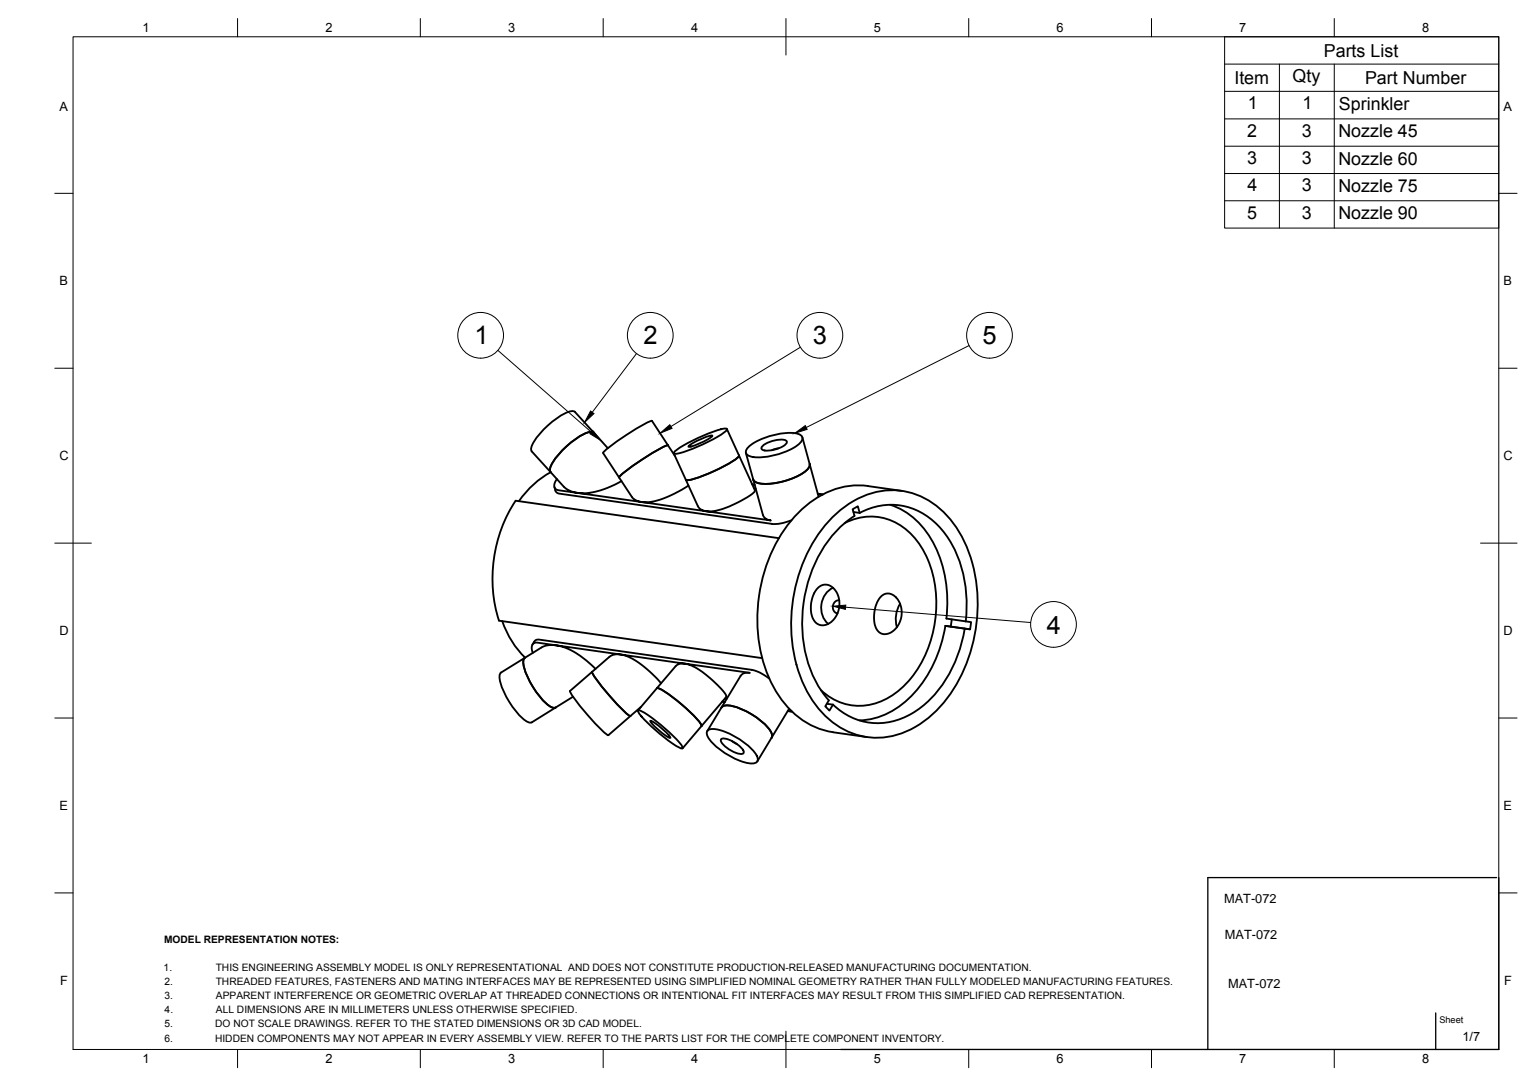
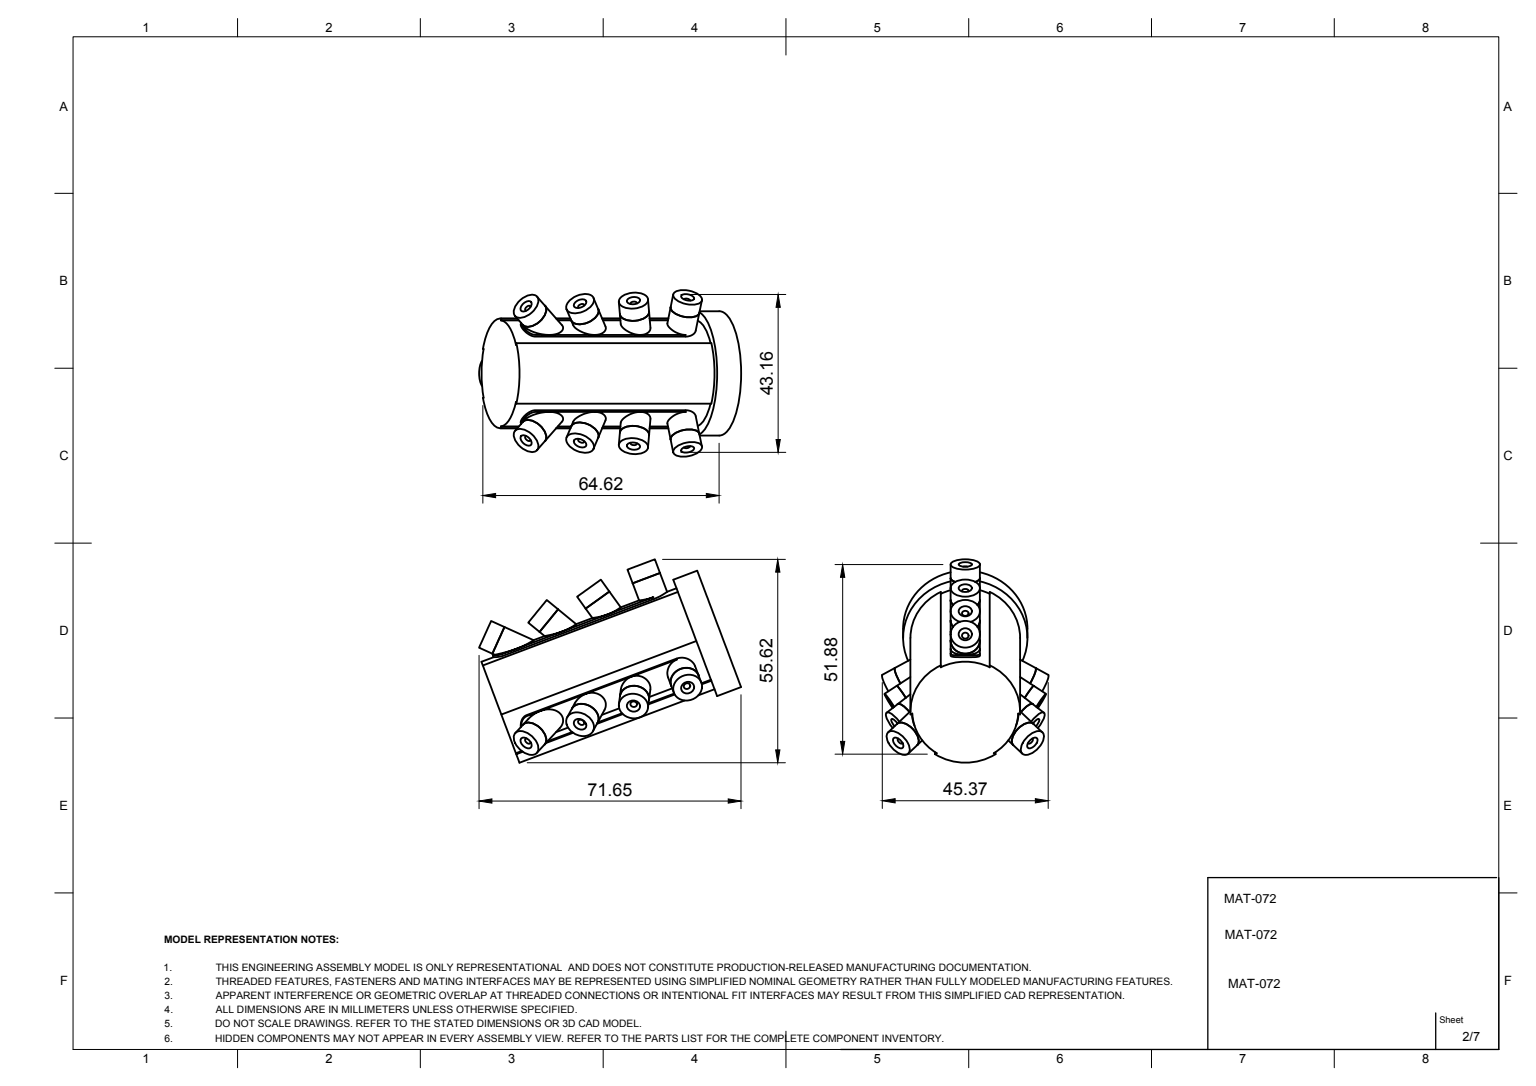
ISO-10303-21;
HEADER;
/* Generated by software containing ST-Developer
 * from STEP Tools, Inc. (www.steptools.com) 
 */

FILE_DESCRIPTION(
/* description */ (''),
/* implementation_level */ '2;1');

FILE_NAME(
/* name */ 'MAT-072',
/* time_stamp */ '2026-10-24T10:30:45-07:00',
/* author */ (''),
/* organization */ (''),
/* preprocessor_version */ 'ST-DEVELOPER v20.2',
/* originating_system */ 'Autodesk Translation Framework v15.15.0.0',
/* authorisation */ '');

FILE_SCHEMA (('AUTOMOTIVE_DESIGN { 1 0 10303 214 3 1 1 }'));
ENDSEC;

DATA;
#10=MECHANICAL_DESIGN_GEOMETRIC_PRESENTATION_REPRESENTATION('',(#77,#78,
#79,#80,#81),#5183);
#11=ITEM_DEFINED_TRANSFORMATION($,$,#2425,#2665);
#12=ITEM_DEFINED_TRANSFORMATION($,$,#2605,#2666);
#13=ITEM_DEFINED_TRANSFORMATION($,$,#2620,#2667);
#14=ITEM_DEFINED_TRANSFORMATION($,$,#2635,#2668);
#15=ITEM_DEFINED_TRANSFORMATION($,$,#2650,#2669);
#16=ITEM_DEFINED_TRANSFORMATION($,$,#2605,#2670);
#17=ITEM_DEFINED_TRANSFORMATION($,$,#2605,#2671);
#18=ITEM_DEFINED_TRANSFORMATION($,$,#2620,#2672);
#19=ITEM_DEFINED_TRANSFORMATION($,$,#2620,#2673);
#20=ITEM_DEFINED_TRANSFORMATION($,$,#2635,#2674);
#21=ITEM_DEFINED_TRANSFORMATION($,$,#2635,#2675);
#22=ITEM_DEFINED_TRANSFORMATION($,$,#2650,#2676);
#23=ITEM_DEFINED_TRANSFORMATION($,$,#2650,#2677);
#24=(
REPRESENTATION_RELATIONSHIP($,$,#5214,#5213)
REPRESENTATION_RELATIONSHIP_WITH_TRANSFORMATION(#11)
SHAPE_REPRESENTATION_RELATIONSHIP()
);
#25=(
REPRESENTATION_RELATIONSHIP($,$,#5215,#5213)
REPRESENTATION_RELATIONSHIP_WITH_TRANSFORMATION(#12)
SHAPE_REPRESENTATION_RELATIONSHIP()
);
#26=(
REPRESENTATION_RELATIONSHIP($,$,#5216,#5213)
REPRESENTATION_RELATIONSHIP_WITH_TRANSFORMATION(#13)
SHAPE_REPRESENTATION_RELATIONSHIP()
);
#27=(
REPRESENTATION_RELATIONSHIP($,$,#5217,#5213)
REPRESENTATION_RELATIONSHIP_WITH_TRANSFORMATION(#14)
SHAPE_REPRESENTATION_RELATIONSHIP()
);
#28=(
REPRESENTATION_RELATIONSHIP($,$,#5218,#5213)
REPRESENTATION_RELATIONSHIP_WITH_TRANSFORMATION(#15)
SHAPE_REPRESENTATION_RELATIONSHIP()
);
#29=(
REPRESENTATION_RELATIONSHIP($,$,#5215,#5213)
REPRESENTATION_RELATIONSHIP_WITH_TRANSFORMATION(#16)
SHAPE_REPRESENTATION_RELATIONSHIP()
);
#30=(
REPRESENTATION_RELATIONSHIP($,$,#5215,#5213)
REPRESENTATION_RELATIONSHIP_WITH_TRANSFORMATION(#17)
SHAPE_REPRESENTATION_RELATIONSHIP()
);
#31=(
REPRESENTATION_RELATIONSHIP($,$,#5216,#5213)
REPRESENTATION_RELATIONSHIP_WITH_TRANSFORMATION(#18)
SHAPE_REPRESENTATION_RELATIONSHIP()
);
#32=(
REPRESENTATION_RELATIONSHIP($,$,#5216,#5213)
REPRESENTATION_RELATIONSHIP_WITH_TRANSFORMATION(#19)
SHAPE_REPRESENTATION_RELATIONSHIP()
);
#33=(
REPRESENTATION_RELATIONSHIP($,$,#5217,#5213)
REPRESENTATION_RELATIONSHIP_WITH_TRANSFORMATION(#20)
SHAPE_REPRESENTATION_RELATIONSHIP()
);
#34=(
REPRESENTATION_RELATIONSHIP($,$,#5217,#5213)
REPRESENTATION_RELATIONSHIP_WITH_TRANSFORMATION(#21)
SHAPE_REPRESENTATION_RELATIONSHIP()
);
#35=(
REPRESENTATION_RELATIONSHIP($,$,#5218,#5213)
REPRESENTATION_RELATIONSHIP_WITH_TRANSFORMATION(#22)
SHAPE_REPRESENTATION_RELATIONSHIP()
);
#36=(
REPRESENTATION_RELATIONSHIP($,$,#5218,#5213)
REPRESENTATION_RELATIONSHIP_WITH_TRANSFORMATION(#23)
SHAPE_REPRESENTATION_RELATIONSHIP()
);
#37=CONTEXT_DEPENDENT_SHAPE_REPRESENTATION(#24,#5200);
#38=CONTEXT_DEPENDENT_SHAPE_REPRESENTATION(#25,#5201);
#39=CONTEXT_DEPENDENT_SHAPE_REPRESENTATION(#26,#5202);
#40=CONTEXT_DEPENDENT_SHAPE_REPRESENTATION(#27,#5203);
#41=CONTEXT_DEPENDENT_SHAPE_REPRESENTATION(#28,#5204);
#42=CONTEXT_DEPENDENT_SHAPE_REPRESENTATION(#29,#5205);
#43=CONTEXT_DEPENDENT_SHAPE_REPRESENTATION(#30,#5206);
#44=CONTEXT_DEPENDENT_SHAPE_REPRESENTATION(#31,#5207);
#45=CONTEXT_DEPENDENT_SHAPE_REPRESENTATION(#32,#5208);
#46=CONTEXT_DEPENDENT_SHAPE_REPRESENTATION(#33,#5209);
#47=CONTEXT_DEPENDENT_SHAPE_REPRESENTATION(#34,#5210);
#48=CONTEXT_DEPENDENT_SHAPE_REPRESENTATION(#35,#5211);
#49=CONTEXT_DEPENDENT_SHAPE_REPRESENTATION(#36,#5212);
#50=NEXT_ASSEMBLY_USAGE_OCCURRENCE('Sprinkler:1','Sprinkler:1',
'Sprinkler:1',#5220,#5221,'Sprinkler:1');
#51=NEXT_ASSEMBLY_USAGE_OCCURRENCE('Nozzle 45:1','Nozzle 45:1',
'Nozzle 45:1',#5220,#5222,'Nozzle 45:1');
#52=NEXT_ASSEMBLY_USAGE_OCCURRENCE('Nozzle 60:1','Nozzle 60:1',
'Nozzle 60:1',#5220,#5223,'Nozzle 60:1');
#53=NEXT_ASSEMBLY_USAGE_OCCURRENCE('Nozzle 75:1','Nozzle 75:1',
'Nozzle 75:1',#5220,#5224,'Nozzle 75:1');
#54=NEXT_ASSEMBLY_USAGE_OCCURRENCE('Nozzle 90:1','Nozzle 90:1',
'Nozzle 90:1',#5220,#5225,'Nozzle 90:1');
#55=NEXT_ASSEMBLY_USAGE_OCCURRENCE('Nozzle 45:2','Nozzle 45:2',
'Nozzle 45:2',#5220,#5222,'Nozzle 45:2');
#56=NEXT_ASSEMBLY_USAGE_OCCURRENCE('Nozzle 45:3','Nozzle 45:3',
'Nozzle 45:3',#5220,#5222,'Nozzle 45:3');
#57=NEXT_ASSEMBLY_USAGE_OCCURRENCE('Nozzle 60:2','Nozzle 60:2',
'Nozzle 60:2',#5220,#5223,'Nozzle 60:2');
#58=NEXT_ASSEMBLY_USAGE_OCCURRENCE('Nozzle 60:3','Nozzle 60:3',
'Nozzle 60:3',#5220,#5223,'Nozzle 60:3');
#59=NEXT_ASSEMBLY_USAGE_OCCURRENCE('Nozzle 75:2','Nozzle 75:2',
'Nozzle 75:2',#5220,#5224,'Nozzle 75:2');
#60=NEXT_ASSEMBLY_USAGE_OCCURRENCE('Nozzle 75:3','Nozzle 75:3',
'Nozzle 75:3',#5220,#5224,'Nozzle 75:3');
#61=NEXT_ASSEMBLY_USAGE_OCCURRENCE('Nozzle 90:2','Nozzle 90:2',
'Nozzle 90:2',#5220,#5225,'Nozzle 90:2');
#62=NEXT_ASSEMBLY_USAGE_OCCURRENCE('Nozzle 90:3','Nozzle 90:3',
'Nozzle 90:3',#5220,#5225,'Nozzle 90:3');
#63=CONICAL_SURFACE('',#2616,1.8,0.785398163397447);
#64=CONICAL_SURFACE('',#2631,1.8,0.785398163397439);
#65=CONICAL_SURFACE('',#2646,1.80000000000001,0.785398163397454);
#66=CONICAL_SURFACE('',#2661,1.8,0.785398163397448);
#67=SHAPE_REPRESENTATION_RELATIONSHIP('SRR','None',#5214,#72);
#68=SHAPE_REPRESENTATION_RELATIONSHIP('SRR','None',#5215,#73);
#69=SHAPE_REPRESENTATION_RELATIONSHIP('SRR','None',#5216,#74);
#70=SHAPE_REPRESENTATION_RELATIONSHIP('SRR','None',#5217,#75);
#71=SHAPE_REPRESENTATION_RELATIONSHIP('SRR','None',#5218,#76);
#72=ADVANCED_BREP_SHAPE_REPRESENTATION('',(#82),#5178);
#73=ADVANCED_BREP_SHAPE_REPRESENTATION('',(#83),#5179);
#74=ADVANCED_BREP_SHAPE_REPRESENTATION('',(#84),#5180);
#75=ADVANCED_BREP_SHAPE_REPRESENTATION('',(#85),#5181);
#76=ADVANCED_BREP_SHAPE_REPRESENTATION('',(#86),#5182);
#77=STYLED_ITEM('',(#5247),#82);
#78=STYLED_ITEM('',(#5247),#83);
#79=STYLED_ITEM('',(#5247),#84);
#80=STYLED_ITEM('',(#5247),#85);
#81=STYLED_ITEM('',(#5247),#86);
#82=MANIFOLD_SOLID_BREP('Sprinkler',#2363);
#83=MANIFOLD_SOLID_BREP('Nozzle 45',#2364);
#84=MANIFOLD_SOLID_BREP('Nozzle 60',#2365);
#85=MANIFOLD_SOLID_BREP('Nozzle 75',#2366);
#86=MANIFOLD_SOLID_BREP('Nozzle 90',#2367);
#87=B_SPLINE_SURFACE_WITH_KNOTS('',3,1,((#4861,#4862),(#4863,#4864),(#4865,
#4866),(#4867,#4868),(#4869,#4870),(#4871,#4872),(#4873,#4874),(#4875,#4876),
(#4877,#4878),(#4879,#4880),(#4881,#4882)),.UNSPECIFIED.,.F.,.F.,.F.,(4,
1,1,1,1,1,1,1,4),(2,2),(3.14159265358979,3.53429173528852,3.92699081698724,
4.31968989868597,4.71238898038469,5.10508806208341,5.49778714378214,5.89048622548086,
6.28318530717959),(0.,0.129347179873149),.UNSPECIFIED.);
#88=B_SPLINE_SURFACE_WITH_KNOTS('',3,1,((#4924,#4925),(#4926,#4927),(#4928,
#4929),(#4930,#4931),(#4932,#4933),(#4934,#4935),(#4936,#4937),(#4938,#4939),
(#4940,#4941),(#4942,#4943),(#4944,#4945)),.UNSPECIFIED.,.F.,.F.,.F.,(4,
1,1,1,1,1,1,1,4),(2,2),(3.14159265358979,3.53429173528851,3.92699081698724,
4.31968989868596,4.71238898038469,5.10508806208341,5.49778714378214,5.89048622548086,
6.28318530717959),(0.,0.129347179873148),.UNSPECIFIED.);
#89=B_SPLINE_SURFACE_WITH_KNOTS('',3,1,((#4987,#4988),(#4989,#4990),(#4991,
#4992),(#4993,#4994),(#4995,#4996),(#4997,#4998),(#4999,#5000),(#5001,#5002),
(#5003,#5004),(#5005,#5006),(#5007,#5008)),.UNSPECIFIED.,.F.,.F.,.F.,(4,
1,1,1,1,1,1,1,4),(2,2),(3.14159265358979,3.53429173528851,3.92699081698723,
4.31968989868596,4.71238898038468,5.10508806208341,5.49778714378213,5.89048622548085,
6.28318530717958),(0.,0.129347179873145),.UNSPECIFIED.);
#90=FACE_BOUND('',#431,.T.);
#91=FACE_BOUND('',#433,.T.);
#92=FACE_BOUND('',#436,.T.);
#93=FACE_BOUND('',#439,.T.);
#94=FACE_BOUND('',#442,.T.);
#95=FACE_BOUND('',#445,.T.);
#96=FACE_BOUND('',#448,.T.);
#97=FACE_BOUND('',#451,.T.);
#98=FACE_BOUND('',#454,.T.);
#99=FACE_BOUND('',#457,.T.);
#100=FACE_BOUND('',#460,.T.);
#101=FACE_BOUND('',#461,.T.);
#102=FACE_BOUND('',#462,.T.);
#103=FACE_BOUND('',#463,.T.);
#104=FACE_BOUND('',#464,.T.);
#105=FACE_BOUND('',#465,.T.);
#106=FACE_BOUND('',#466,.T.);
#107=FACE_BOUND('',#467,.T.);
#108=FACE_BOUND('',#468,.T.);
#109=FACE_BOUND('',#469,.T.);
#110=FACE_BOUND('',#470,.T.);
#111=FACE_BOUND('',#471,.T.);
#112=FACE_BOUND('',#474,.T.);
#113=FACE_BOUND('',#481,.T.);
#114=FACE_BOUND('',#484,.T.);
#115=FACE_BOUND('',#487,.T.);
#116=FACE_BOUND('',#490,.T.);
#117=FACE_BOUND('',#493,.T.);
#118=FACE_BOUND('',#496,.T.);
#119=FACE_BOUND('',#499,.T.);
#120=FACE_BOUND('',#502,.T.);
#121=FACE_BOUND('',#513,.T.);
#122=FACE_BOUND('',#516,.T.);
#123=FACE_BOUND('',#519,.T.);
#124=FACE_BOUND('',#522,.T.);
#125=FACE_BOUND('',#525,.T.);
#126=FACE_BOUND('',#528,.T.);
#127=FACE_BOUND('',#531,.T.);
#128=FACE_BOUND('',#534,.T.);
#129=FACE_BOUND('',#542,.T.);
#130=FACE_BOUND('',#549,.T.);
#131=FACE_BOUND('',#556,.T.);
#132=FACE_BOUND('',#568,.T.);
#133=FACE_BOUND('',#570,.T.);
#134=FACE_BOUND('',#574,.T.);
#135=FACE_BOUND('',#578,.T.);
#136=FACE_BOUND('',#580,.T.);
#137=FACE_BOUND('',#584,.T.);
#138=FACE_BOUND('',#588,.T.);
#139=FACE_BOUND('',#590,.T.);
#140=FACE_BOUND('',#594,.T.);
#141=FACE_BOUND('',#598,.T.);
#142=FACE_BOUND('',#600,.T.);
#143=FACE_BOUND('',#604,.T.);
#144=PLANE('',#2456);
#145=PLANE('',#2461);
#146=PLANE('',#2464);
#147=PLANE('',#2466);
#148=PLANE('',#2470);
#149=PLANE('',#2474);
#150=PLANE('',#2478);
#151=PLANE('',#2482);
#152=PLANE('',#2486);
#153=PLANE('',#2490);
#154=PLANE('',#2494);
#155=PLANE('',#2500);
#156=PLANE('',#2501);
#157=PLANE('',#2509);
#158=PLANE('',#2513);
#159=PLANE('',#2517);
#160=PLANE('',#2521);
#161=PLANE('',#2525);
#162=PLANE('',#2529);
#163=PLANE('',#2533);
#164=PLANE('',#2537);
#165=PLANE('',#2557);
#166=PLANE('',#2560);
#167=PLANE('',#2563);
#168=PLANE('',#2566);
#169=PLANE('',#2569);
#170=PLANE('',#2572);
#171=PLANE('',#2575);
#172=PLANE('',#2578);
#173=PLANE('',#2581);
#174=PLANE('',#2582);
#175=PLANE('',#2583);
#176=PLANE('',#2584);
#177=PLANE('',#2586);
#178=PLANE('',#2587);
#179=PLANE('',#2588);
#180=PLANE('',#2589);
#181=PLANE('',#2591);
#182=PLANE('',#2592);
#183=PLANE('',#2593);
#184=PLANE('',#2594);
#185=PLANE('',#2596);
#186=PLANE('',#2597);
#187=PLANE('',#2598);
#188=PLANE('',#2599);
#189=PLANE('',#2600);
#190=PLANE('',#2601);
#191=PLANE('',#2602);
#192=PLANE('',#2603);
#193=PLANE('',#2604);
#194=PLANE('',#2609);
#195=PLANE('',#2611);
#196=PLANE('',#2617);
#197=PLANE('',#2624);
#198=PLANE('',#2626);
#199=PLANE('',#2632);
#200=PLANE('',#2639);
#201=PLANE('',#2641);
#202=PLANE('',#2647);
#203=PLANE('',#2654);
#204=PLANE('',#2656);
#205=PLANE('',#2662);
#206=B_SPLINE_CURVE_WITH_KNOTS('',3,(#3370,#3371,#3372,#3373,#3374,#3375,
#3376,#3377),.UNSPECIFIED.,.F.,.F.,(4,2,2,4),(0.801601659973552,0.908686694681274,
1.06147652934293,1.21426636400458),.UNSPECIFIED.);
#207=B_SPLINE_CURVE_WITH_KNOTS('',3,(#3379,#3380,#3381,#3382,#3383,#3384,
#3385,#3386,#3387,#3388,#3389,#3390,#3391,#3392),.UNSPECIFIED.,.F.,.F.,
(4,2,2,2,2,2,4),(0.,0.152789834661652,0.305579669323305,0.456356425662796,
0.607133182002287,0.757909938341781,0.801601659973552),.UNSPECIFIED.);
#208=B_SPLINE_CURVE_WITH_KNOTS('',3,(#3396,#3397,#3398,#3399,#3400,#3401,
#3402,#3403,#3404,#3405,#3406,#3407,#3408,#3409,#3410,#3411),
 .UNSPECIFIED.,.F.,.F.,(4,2,2,2,2,2,2,4),(1.41258149283994,1.51470567835646,
1.66615965590029,1.81761363344413,1.96906761098797,2.12052158853181,2.27200321656199,
2.42348484459217),.UNSPECIFIED.);
#209=B_SPLINE_CURVE_WITH_KNOTS('',3,(#3412,#3413,#3414,#3415,#3416,#3417),
 .UNSPECIFIED.,.F.,.F.,(4,2,4),(1.21174242229609,1.36322405032627,1.41258149283994),
 .UNSPECIFIED.);
#210=B_SPLINE_CURVE_WITH_KNOTS('',3,(#3422,#3423,#3424,#3425,#3426,#3427,
#3428,#3429),.UNSPECIFIED.,.F.,.F.,(4,2,2,4),(0.810459053731311,0.931112082660273,
1.09792489409666,1.26473770553305),.UNSPECIFIED.);
#211=B_SPLINE_CURVE_WITH_KNOTS('',3,(#3431,#3432,#3433,#3434,#3435,#3436,
#3437,#3438,#3439,#3440,#3441,#3442,#3443,#3444),.UNSPECIFIED.,.F.,.F.,
(4,2,2,2,2,2,4),(0.,0.166812811436392,0.333625622872784,0.482997237819655,
0.632368852766526,0.781740467713401,0.810459053731311),.UNSPECIFIED.);
#212=B_SPLINE_CURVE_WITH_KNOTS('',3,(#3446,#3447,#3448,#3449,#3450,#3451,
#3452,#3453,#3454,#3455,#3456,#3457,#3458,#3459,#3460,#3461,#3462,#3463),
 .UNSPECIFIED.,.F.,.F.,(4,2,2,2,2,2,2,2,4),(1.21426636400458,1.37281902636882,
1.53137168873306,1.68587949128402,1.84038729383497,1.99489509638593,2.14940289893689,
2.30795556130114,2.46650822366539),.UNSPECIFIED.);
#213=B_SPLINE_CURVE_WITH_KNOTS('',3,(#3468,#3469,#3470,#3471,#3472,#3473,
#3474,#3475,#3476,#3477),.UNSPECIFIED.,.F.,.F.,(4,2,2,2,4),(0.84921255840186,
0.855460999411689,1.0133776521287,1.20423317275903,1.39508869338936),
 .UNSPECIFIED.);
#214=B_SPLINE_CURVE_WITH_KNOTS('',3,(#3479,#3480,#3481,#3482,#3483,#3484,
#3485,#3486,#3487,#3488,#3489,#3490),.UNSPECIFIED.,.F.,.F.,(4,2,2,2,2,4),
(0.,0.19085552063033,0.38171104126066,0.539627693977667,0.697544346694674,
0.84921255840186),.UNSPECIFIED.);
#215=B_SPLINE_CURVE_WITH_KNOTS('',3,(#3492,#3493,#3494,#3495,#3496,#3497,
#3498,#3499,#3500,#3501,#3502,#3503,#3504,#3505,#3506,#3507,#3508,#3509),
 .UNSPECIFIED.,.F.,.F.,(4,2,2,2,2,2,2,2,4),(1.26473770553305,1.44115993597425,
1.61758216641546,1.77878219205947,1.93998221770349,2.10118224334752,2.26238226899155,
2.43880449943275,2.61522672987395),.UNSPECIFIED.);
#216=B_SPLINE_CURVE_WITH_KNOTS('',3,(#3513,#3514,#3515,#3516,#3517,#3518,
#3519,#3520,#3521,#3522,#3523,#3524,#3525,#3526,#3527,#3528,#3529,#3530,
#3531,#3532,#3533,#3534),.UNSPECIFIED.,.F.,.F.,(4,2,2,2,2,2,2,2,2,2,4),
(1.39508869338936,1.63068735474474,1.86628601610013,2.01895939966093,2.09529609144134,
2.17163278322174,2.24796947500215,2.32430616678255,2.47697955034337,2.71257821169876,
2.94817687305416),.UNSPECIFIED.);
#217=B_SPLINE_CURVE_WITH_KNOTS('',3,(#3537,#3538,#3539,#3540,#3541,#3542,
#3543,#3544,#3545,#3546,#3547,#3548,#3549,#3550,#3551,#3552,#3553,#3554,
#3555,#3556,#3557,#3558,#3559,#3560,#3561,#3562),.UNSPECIFIED.,.F.,.F.,
(4,2,2,2,2,2,2,2,2,2,2,2,4),(0.,0.0444658256706816,0.109825747467382,0.210987273969983,
0.363115011869221,0.476603266918211,0.543343022865724,0.610052308554092,
0.7232875236507,0.87579543247345,0.97697424211648,1.04237097445545,1.08685368328188),
 .UNSPECIFIED.);
#218=B_SPLINE_CURVE_WITH_KNOTS('',3,(#3577,#3578,#3579,#3580,#3581,#3582,
#3583,#3584),.UNSPECIFIED.,.F.,.F.,(4,2,2,4),(0.801601659973551,0.908686694681269,
1.06147652934292,1.21426636400457),.UNSPECIFIED.);
#219=B_SPLINE_CURVE_WITH_KNOTS('',3,(#3586,#3587,#3588,#3589,#3590,#3591,
#3592,#3593,#3594,#3595,#3596,#3597,#3598,#3599),.UNSPECIFIED.,.F.,.F.,
(4,2,2,2,2,2,4),(0.,0.152789834661651,0.305579669323302,0.456356425662796,
0.607133182002289,0.757909938341779,0.801601659973551),.UNSPECIFIED.);
#220=B_SPLINE_CURVE_WITH_KNOTS('',3,(#3603,#3604,#3605,#3606,#3607,#3608,
#3609,#3610,#3611,#3612,#3613,#3614,#3615,#3616,#3617,#3618),
 .UNSPECIFIED.,.F.,.F.,(4,2,2,2,2,2,2,4),(1.41258149283993,1.51470567835645,
1.66615965590029,1.81761363344413,1.96906761098797,2.1205215885318,2.27200321656199,
2.42348484459217),.UNSPECIFIED.);
#221=B_SPLINE_CURVE_WITH_KNOTS('',3,(#3619,#3620,#3621,#3622,#3623,#3624),
 .UNSPECIFIED.,.F.,.F.,(4,2,4),(1.21174242229609,1.36322405032627,1.41258149283993),
 .UNSPECIFIED.);
#222=B_SPLINE_CURVE_WITH_KNOTS('',3,(#3629,#3630,#3631,#3632,#3633,#3634,
#3635,#3636),.UNSPECIFIED.,.F.,.F.,(4,2,2,4),(0.810459053731318,0.931112082660271,
1.09792489409666,1.26473770553306),.UNSPECIFIED.);
#223=B_SPLINE_CURVE_WITH_KNOTS('',3,(#3638,#3639,#3640,#3641,#3642,#3643,
#3644,#3645,#3646,#3647,#3648,#3649,#3650,#3651),.UNSPECIFIED.,.F.,.F.,
(4,2,2,2,2,2,4),(0.,0.166812811436393,0.333625622872785,0.482997237819654,
0.632368852766523,0.781740467713397,0.810459053731318),.UNSPECIFIED.);
#224=B_SPLINE_CURVE_WITH_KNOTS('',3,(#3653,#3654,#3655,#3656,#3657,#3658,
#3659,#3660,#3661,#3662,#3663,#3664,#3665,#3666,#3667,#3668,#3669,#3670),
 .UNSPECIFIED.,.F.,.F.,(4,2,2,2,2,2,2,2,4),(1.21426636400457,1.37281902636881,
1.53137168873306,1.68587949128401,1.84038729383497,1.99489509638593,2.14940289893689,
2.30795556130114,2.46650822366538),.UNSPECIFIED.);
#225=B_SPLINE_CURVE_WITH_KNOTS('',3,(#3675,#3676,#3677,#3678,#3679,#3680,
#3681,#3682),.UNSPECIFIED.,.F.,.F.,(4,2,2,4),(0.848478832255458,0.991796836691898,
1.19347267089766,1.39514850510343),.UNSPECIFIED.);
#226=B_SPLINE_CURVE_WITH_KNOTS('',3,(#3684,#3685,#3686,#3687,#3688,#3689,
#3690,#3691,#3692,#3693,#3694,#3695,#3696,#3697),.UNSPECIFIED.,.F.,.F.,
(4,2,2,2,2,2,4),(0.,0.201675834205757,0.403351668411514,0.550462960481608,
0.697574252551703,0.8446855446218,0.848478832255458),.UNSPECIFIED.);
#227=B_SPLINE_CURVE_WITH_KNOTS('',3,(#3699,#3700,#3701,#3702,#3703,#3704,
#3705,#3706,#3707,#3708,#3709,#3710,#3711,#3712,#3713,#3714,#3715,#3716),
 .UNSPECIFIED.,.F.,.F.,(4,2,2,2,2,2,2,2,4),(1.26473770553306,1.44115993597426,
1.61758216641546,1.77878219205948,1.93998221770349,2.10118224334752,2.26238226899154,
2.43880449943275,2.61522672987395),.UNSPECIFIED.);
#228=B_SPLINE_CURVE_WITH_KNOTS('',3,(#3720,#3721,#3722,#3723,#3724,#3725,
#3726,#3727,#3728,#3729,#3730,#3731,#3732,#3733,#3734,#3735,#3736,#3737,
#3738,#3739,#3740,#3741),.UNSPECIFIED.,.F.,.F.,(4,2,2,2,2,2,2,2,2,2,4),
(1.39514850510343,1.60860320712188,1.82205790914033,1.99791237111712,2.08583960210551,
2.17376683309391,2.26169406408231,2.34962129507071,2.5254757570475,2.73893045906596,
2.95238516108442),.UNSPECIFIED.);
#229=B_SPLINE_CURVE_WITH_KNOTS('',3,(#3744,#3745,#3746,#3747,#3748,#3749,
#3750,#3751,#3752,#3753,#3754,#3755,#3756,#3757,#3758,#3759,#3760,#3761,
#3762,#3763,#3764,#3765,#3766,#3767,#3768,#3769),.UNSPECIFIED.,.F.,.F.,
(4,2,2,2,2,2,2,2,2,2,2,2,4),(0.,0.0444658256707017,0.109825747467453,0.210987273970143,
0.363115011869592,0.4766032669186,0.543343022866364,0.610052308555067,0.723287523653244,
0.875795432478097,0.97697424212264,1.04237097446268,1.08685368328966),
 .UNSPECIFIED.);
#230=B_SPLINE_CURVE_WITH_KNOTS('',3,(#3775,#3776,#3777,#3778,#3779,#3780,
#3781,#3782),.UNSPECIFIED.,.F.,.F.,(4,2,2,4),(0.80160165997355,0.908686694681275,
1.06147652934293,1.21426636400458),.UNSPECIFIED.);
#231=B_SPLINE_CURVE_WITH_KNOTS('',3,(#3784,#3785,#3786,#3787,#3788,#3789,
#3790,#3791,#3792,#3793,#3794,#3795,#3796,#3797),.UNSPECIFIED.,.F.,.F.,
(4,2,2,2,2,2,4),(0.,0.152789834661653,0.305579669323305,0.456356425662799,
0.607133182002292,0.757909938341784,0.80160165997355),.UNSPECIFIED.);
#232=B_SPLINE_CURVE_WITH_KNOTS('',3,(#3801,#3802,#3803,#3804,#3805,#3806,
#3807,#3808,#3809,#3810,#3811,#3812,#3813,#3814,#3815,#3816),
 .UNSPECIFIED.,.F.,.F.,(4,2,2,2,2,2,2,4),(1.41258149283993,1.51470567835645,
1.66615965590029,1.81761363344413,1.96906761098797,2.12052158853181,2.27200321656199,
2.42348484459217),.UNSPECIFIED.);
#233=B_SPLINE_CURVE_WITH_KNOTS('',3,(#3817,#3818,#3819,#3820,#3821,#3822),
 .UNSPECIFIED.,.F.,.F.,(4,2,4),(1.21174242229609,1.36322405032627,1.41258149283993),
 .UNSPECIFIED.);
#234=B_SPLINE_CURVE_WITH_KNOTS('',3,(#3827,#3828,#3829,#3830,#3831,#3832,
#3833,#3834),.UNSPECIFIED.,.F.,.F.,(4,2,2,4),(0.810451797988797,0.931104826917751,
1.09791763835414,1.26473044979053),.UNSPECIFIED.);
#235=B_SPLINE_CURVE_WITH_KNOTS('',3,(#3836,#3837,#3838,#3839,#3840,#3841,
#3842,#3843,#3844,#3845,#3846,#3847,#3848,#3849),.UNSPECIFIED.,.F.,.F.,
(4,2,2,2,2,2,4),(0.,0.163827053405726,0.327654106811452,0.48000785191773,
0.632361597024009,0.781733211970881,0.810451797988797),.UNSPECIFIED.);
#236=B_SPLINE_CURVE_WITH_KNOTS('',3,(#3851,#3852,#3853,#3854,#3855,#3856,
#3857,#3858,#3859,#3860,#3861,#3862,#3863,#3864,#3865,#3866,#3867,#3868),
 .UNSPECIFIED.,.F.,.F.,(4,2,2,2,2,2,2,2,4),(1.21426636400458,1.37281902636882,
1.53137168873306,1.68587949128402,1.84038729383497,1.99489509638594,2.1494028989369,
2.30795556130114,2.46650822366539),.UNSPECIFIED.);
#237=B_SPLINE_CURVE_WITH_KNOTS('',3,(#3873,#3874,#3875,#3876,#3877,#3878,
#3879,#3880,#3881,#3882),.UNSPECIFIED.,.F.,.F.,(4,2,2,2,4),(0.849212558401863,
0.855460999411694,1.01337765212871,1.20423317275904,1.39508869338936),
 .UNSPECIFIED.);
#238=B_SPLINE_CURVE_WITH_KNOTS('',3,(#3884,#3885,#3886,#3887,#3888,#3889,
#3890,#3891,#3892,#3893,#3894,#3895),.UNSPECIFIED.,.F.,.F.,(4,2,2,2,2,4),
(0.,0.190855520630331,0.381711041260663,0.539627693977671,0.697544346694678,
0.849212558401863),.UNSPECIFIED.);
#239=B_SPLINE_CURVE_WITH_KNOTS('',3,(#3897,#3898,#3899,#3900,#3901,#3902,
#3903,#3904,#3905,#3906,#3907,#3908,#3909,#3910,#3911,#3912,#3913,#3914),
 .UNSPECIFIED.,.F.,.F.,(4,2,2,2,2,2,2,2,4),(1.26473044979053,1.45047293867533,
1.63621542756013,1.78793284105988,1.93965025455964,2.0913676680594,2.24308508155916,
2.42882757044396,2.61457005932877),.UNSPECIFIED.);
#240=B_SPLINE_CURVE_WITH_KNOTS('',3,(#3918,#3919,#3920,#3921,#3922,#3923,
#3924,#3925,#3926,#3927,#3928,#3929,#3930,#3931,#3932,#3933,#3934,#3935,
#3936,#3937,#3938,#3939),.UNSPECIFIED.,.F.,.F.,(4,2,2,2,2,2,2,2,2,2,4),
(1.39508869338936,1.63068735474475,1.86628601610013,2.01895939966094,2.09529609144135,
2.17163278322175,2.24796947500216,2.32430616678257,2.47697955034339,2.71257821169878,
2.94817687305417),.UNSPECIFIED.);
#241=B_SPLINE_CURVE_WITH_KNOTS('',3,(#3942,#3943,#3944,#3945,#3946,#3947,
#3948,#3949,#3950,#3951,#3952,#3953,#3954,#3955,#3956,#3957,#3958,#3959,
#3960,#3961,#3962,#3963,#3964,#3965,#3966,#3967),.UNSPECIFIED.,.F.,.F.,
(4,2,2,2,2,2,2,2,2,2,2,2,4),(0.,0.0444658256707104,0.109825747467599,0.210987273970278,
0.3631150118696,0.476603266918339,0.54334302286555,0.610052308553677,0.723287523650531,
0.875795432473984,0.97697424211741,1.0423709744566,1.08685368328313),
 .UNSPECIFIED.);
#242=B_SPLINE_CURVE_WITH_KNOTS('',3,(#4068,#4069,#4070,#4071,#4072,#4073,
#4074,#4075,#4076,#4077,#4078,#4079,#4080,#4081,#4082,#4083,#4084,#4085),
 .UNSPECIFIED.,.F.,.F.,(4,2,2,2,2,2,2,2,4),(-2.42440986895006,-2.27286833474306,
-2.12132680053607,-1.9698171011243,-1.81830740171254,-1.66679770230078,
-1.51528800288901,-1.36374646868202,-1.21220493447502),.UNSPECIFIED.);
#243=B_SPLINE_CURVE_WITH_KNOTS('',3,(#4135,#4136,#4137,#4138,#4139,#4140,
#4141,#4142,#4143,#4144,#4145,#4146,#4147,#4148,#4149,#4150,#4151,#4152,
#4153,#4154,#4155),.UNSPECIFIED.,.F.,.F.,(4,2,2,2,3,2,2,2,2,4),(1.63431795680218,
1.63484051213071,1.74655213492763,1.90358589296679,2.06061965100595,2.19559646985844,
2.33057328871092,2.44200600177385,2.55343871483678,2.66004451397958),
 .UNSPECIFIED.);
#244=B_SPLINE_CURVE_WITH_KNOTS('',3,(#4156,#4157,#4158,#4159,#4160,#4161,
#4162,#4163,#4164,#4165,#4166,#4167,#4168,#4169,#4170,#4171,#4172,#4173,
#4174,#4175,#4176,#4177,#4178,#4179),.UNSPECIFIED.,.F.,.F.,(4,2,2,2,2,2,
2,2,2,2,2,4),(2.66004451397958,2.66487142789972,2.77630414096266,2.91128095981515,
3.04625777866764,3.20329153670679,3.36032529474595,3.47203691754285,3.5278927289413,
3.58374854033975,3.63960435173821,3.69493760780813),.UNSPECIFIED.);
#245=B_SPLINE_CURVE_WITH_KNOTS('',3,(#4182,#4183,#4184,#4185,#4186,#4187,
#4188,#4189,#4190,#4191,#4192,#4193,#4194,#4195,#4196,#4197,#4198,#4199,
#4200,#4201,#4202,#4203,#4204),.UNSPECIFIED.,.F.,.F.,(4,2,2,2,3,2,2,2,2,
2,4),(1.63645246149242,1.6458071028209,1.76735674157733,1.91500283165642,
2.06264892173552,2.21065304350676,2.35865716527801,2.45711954510512,2.55558192493224,
2.65404430475936,2.66124396153498),.UNSPECIFIED.);
#246=B_SPLINE_CURVE_WITH_KNOTS('',3,(#4205,#4206,#4207,#4208,#4209,#4210,
#4211,#4212,#4213,#4214,#4215,#4216,#4217,#4218,#4219,#4220,#4221,#4222,
#4223,#4224,#4225,#4226),.UNSPECIFIED.,.F.,.F.,(4,2,2,2,2,2,2,2,2,2,4),
(2.66124396153498,2.75250668458648,2.90051080635773,3.04851492812899,3.19616101820807,
3.34380710828715,3.46535674704357,3.52613156642178,3.58690638579999,3.64768120517821,
3.69910138322794),.UNSPECIFIED.);
#247=B_SPLINE_CURVE_WITH_KNOTS('',3,(#4229,#4230,#4231,#4232,#4233,#4234,
#4235,#4236,#4237,#4238,#4239,#4240,#4241,#4242,#4243,#4244,#4245,#4246,
#4247,#4248,#4249),.UNSPECIFIED.,.F.,.F.,(4,2,2,3,2,2,2,2,2,4),(1.48658026968319,
1.57668032617585,1.70181043495793,1.82694054374001,1.94229840394621,2.0576562641524,
2.16466765320846,2.27167904226452,2.37869043132058,2.39673280800115),
 .UNSPECIFIED.);
#248=B_SPLINE_CURVE_WITH_KNOTS('',3,(#4250,#4251,#4252,#4253,#4254,#4255,
#4256,#4257,#4258,#4259,#4260,#4261,#4262,#4263,#4264,#4265,#4266,#4267,
#4268,#4269),.UNSPECIFIED.,.F.,.F.,(4,2,2,2,2,2,2,2,2,4),(2.39673280800115,
2.48570182037664,2.60105968058284,2.71641754078903,2.84154764957111,2.96667775835319,
3.07591353624385,3.18514931413451,3.29438509202518,3.3135208134232),
 .UNSPECIFIED.);
#249=B_SPLINE_CURVE_WITH_KNOTS('',3,(#4272,#4273,#4274,#4275,#4276,#4277,
#4278,#4279,#4280,#4281,#4282,#4283,#4284,#4285,#4286,#4287,#4288,#4289,
#4290,#4291,#4292),.UNSPECIFIED.,.F.,.F.,(4,2,2,3,2,2,2,2,2,4),(1.48667142164751,
1.57677147814025,1.70190158692234,1.82703169570442,1.94802136665288,2.06901103760135,
2.17041340390623,2.27181577021112,2.37321813651602,2.39644556681379),
 .UNSPECIFIED.);
#250=B_SPLINE_CURVE_WITH_KNOTS('',3,(#4293,#4294,#4295,#4296,#4297,#4298,
#4299,#4300,#4301,#4302,#4303,#4304,#4305,#4306,#4307,#4308,#4309,#4310,
#4311,#4312),.UNSPECIFIED.,.F.,.F.,(4,2,2,2,2,2,2,2,2,4),(2.39644556681379,
2.47462050282091,2.59561017376938,2.71659984471785,2.84172995349992,2.966860062282,
3.07609584017266,3.18533161806333,3.294567395954,3.31370311735193),
 .UNSPECIFIED.);
#251=B_SPLINE_CURVE_WITH_KNOTS('',3,(#4315,#4316,#4317,#4318,#4319,#4320,
#4321,#4322,#4323,#4324,#4325,#4326,#4327,#4328,#4329,#4330,#4331,#4332,
#4333,#4334,#4335),.UNSPECIFIED.,.F.,.F.,(4,2,2,3,2,2,2,2,2,4),(1.42510602309759,
1.50257240162674,1.61295870334865,1.72334500507057,1.83225417045197,1.94116333583337,
2.04500754168813,2.1488517475429,2.25269595339766,2.2848744256183),
 .UNSPECIFIED.);
#252=B_SPLINE_CURVE_WITH_KNOTS('',3,(#4336,#4337,#4338,#4339,#4340,#4341,
#4342,#4343,#4344,#4345,#4346,#4347,#4348,#4349,#4350,#4351,#4352,#4353,
#4354,#4355),.UNSPECIFIED.,.F.,.F.,(4,2,2,2,2,2,2,2,2,4),(2.2848744256183,
2.35654015925242,2.46544932463382,2.57435849001523,2.68474479173714,2.79513109345905,
2.90282767176861,3.01052425007817,3.11822082838774,3.14845102816816),
 .UNSPECIFIED.);
#253=B_SPLINE_CURVE_WITH_KNOTS('',3,(#4358,#4359,#4360,#4361,#4362,#4363,
#4364,#4365,#4366,#4367,#4368,#4369,#4370,#4371,#4372,#4373,#4374,#4375,
#4376,#4377,#4378),.UNSPECIFIED.,.F.,.F.,(4,2,2,3,2,2,2,2,2,4),(1.42506934481542,
1.50220099251643,1.61276096598296,1.72332093944948,1.83050112648501,1.93768131352053,
2.04324956210919,2.14881781069785,2.25438605928651,2.28497277338716),
 .UNSPECIFIED.);
#254=B_SPLINE_CURVE_WITH_KNOTS('',3,(#4379,#4380,#4381,#4382,#4383,#4384,
#4385,#4386,#4387,#4388,#4389,#4390,#4391,#4392,#4393,#4394,#4395,#4396,
#4397,#4398),.UNSPECIFIED.,.F.,.F.,(4,2,2,2,2,2,2,2,2,4),(2.28497277338716,
2.35995430787517,2.46713449491069,2.57431468194622,2.68487465541274,2.79543462887926,
2.90295645465092,3.01047828042258,3.11800010619425,3.1483902842649),
 .UNSPECIFIED.);
#255=B_SPLINE_CURVE_WITH_KNOTS('',3,(#4401,#4402,#4403,#4404,#4405,#4406,
#4407,#4408,#4409,#4410,#4411,#4412,#4413,#4414,#4415,#4416,#4417,#4418,
#4419,#4420),.UNSPECIFIED.,.F.,.F.,(4,2,2,2,2,2,2,2,2,4),(0.140389663816896,
0.211667950083815,0.317493899242379,0.423319848400943,0.529145797559505,
0.634971746718067,0.740805721759974,0.846639696801881,0.952473671843789,
0.987029360618753),.UNSPECIFIED.);
#256=B_SPLINE_CURVE_WITH_KNOTS('',3,(#4421,#4422,#4423,#4424,#4425,#4426,
#4427,#4428,#4429,#4430,#4431,#4432,#4433,#4434,#4435,#4436,#4437,#4438,
#4439,#4440,#4441),.UNSPECIFIED.,.F.,.F.,(4,2,2,2,2,2,2,3,2,4),(0.987029360618753,
1.0583076468857,1.16413359604426,1.26995954520282,1.37578549436138,1.48161144351995,
1.58744541856186,1.69327939360377,1.79911336864567,1.83366905742066),
 .UNSPECIFIED.);
#257=B_SPLINE_CURVE_WITH_KNOTS('',3,(#4444,#4445,#4446,#4447,#4448,#4449,
#4450,#4451,#4452,#4453,#4454,#4455,#4456,#4457,#4458,#4459,#4460,#4461,
#4462,#4463),.UNSPECIFIED.,.F.,.F.,(4,2,2,2,2,2,2,2,2,4),(0.14038966381692,
0.211667950083817,0.317493899242381,0.423319848400946,0.529145797559508,
0.634971746718069,0.740805721759977,0.846639696801884,0.952473671843792,
0.987029360618756),.UNSPECIFIED.);
#258=B_SPLINE_CURVE_WITH_KNOTS('',3,(#4464,#4465,#4466,#4467,#4468,#4469,
#4470,#4471,#4472,#4473,#4474,#4475,#4476,#4477,#4478,#4479,#4480,#4481,
#4482,#4483,#4484),.UNSPECIFIED.,.F.,.F.,(4,2,2,2,2,2,2,3,2,4),(0.987029360618756,
1.0583076468857,1.16413359604426,1.26995954520282,1.37578549436139,1.48161144351995,
1.58744541856186,1.69327939360377,1.79911336864568,1.83366905742069),
 .UNSPECIFIED.);
#259=B_SPLINE_CURVE_WITH_KNOTS('',3,(#4487,#4488,#4489,#4490,#4491,#4492,
#4493,#4494,#4495,#4496,#4497,#4498,#4499,#4500,#4501,#4502,#4503,#4504,
#4505,#4506,#4507),.UNSPECIFIED.,.F.,.F.,(4,2,2,2,3,2,2,2,2,4),(1.63431795680214,
1.63484051213073,1.74655213492764,1.90358589296679,2.06061965100595,2.19559646985844,
2.33057328871092,2.44200600177386,2.5534387148368,2.66004451397959),
 .UNSPECIFIED.);
#260=B_SPLINE_CURVE_WITH_KNOTS('',3,(#4508,#4509,#4510,#4511,#4512,#4513,
#4514,#4515,#4516,#4517,#4518,#4519,#4520,#4521,#4522,#4523,#4524,#4525,
#4526,#4527,#4528,#4529,#4530,#4531),.UNSPECIFIED.,.F.,.F.,(4,2,2,2,2,2,
2,2,2,2,2,4),(2.66004451397959,2.66487142789973,2.77630414096267,2.91128095981515,
3.04625777866764,3.2032915367068,3.36032529474595,3.47203691754286,3.52789272894132,
3.58374854033977,3.63960435173823,3.69493760780809),.UNSPECIFIED.);
#261=B_SPLINE_CURVE_WITH_KNOTS('',3,(#4534,#4535,#4536,#4537,#4538,#4539,
#4540,#4541,#4542,#4543,#4544,#4545,#4546,#4547,#4548,#4549,#4550,#4551,
#4552,#4553,#4554),.UNSPECIFIED.,.F.,.F.,(4,2,2,3,2,2,2,2,2,4),(1.48658026968317,
1.57668032617585,1.70181043495793,1.82694054374001,1.9422984039462,2.0576562641524,
2.16466765320846,2.27167904226452,2.37869043132058,2.39673280800115),
 .UNSPECIFIED.);
#262=B_SPLINE_CURVE_WITH_KNOTS('',3,(#4555,#4556,#4557,#4558,#4559,#4560,
#4561,#4562,#4563,#4564,#4565,#4566,#4567,#4568,#4569,#4570,#4571,#4572,
#4573,#4574),.UNSPECIFIED.,.F.,.F.,(4,2,2,2,2,2,2,2,2,4),(2.39673280800115,
2.48570182037664,2.60105968058283,2.71641754078903,2.84154764957111,2.96667775835319,
3.07591353624386,3.18514931413453,3.29438509202519,3.31352081342317),
 .UNSPECIFIED.);
#263=B_SPLINE_CURVE_WITH_KNOTS('',3,(#4577,#4578,#4579,#4580,#4581,#4582,
#4583,#4584,#4585,#4586,#4587,#4588,#4589,#4590,#4591,#4592,#4593,#4594,
#4595,#4596,#4597),.UNSPECIFIED.,.F.,.F.,(4,2,2,3,2,2,2,2,2,4),(1.42506934481545,
1.50220099251643,1.61276096598296,1.72332093944948,1.83050112648501,1.93768131352053,
2.04324956210919,2.14881781069785,2.25438605928651,2.28497277338716),
 .UNSPECIFIED.);
#264=B_SPLINE_CURVE_WITH_KNOTS('',3,(#4598,#4599,#4600,#4601,#4602,#4603,
#4604,#4605,#4606,#4607,#4608,#4609,#4610,#4611,#4612,#4613,#4614,#4615,
#4616,#4617),.UNSPECIFIED.,.F.,.F.,(4,2,2,2,2,2,2,2,2,4),(2.28497277338716,
2.35995430787516,2.46713449491069,2.57431468194622,2.68487465541274,2.79543462887926,
2.90295645465092,3.01047828042259,3.11800010619425,3.14839028426493),
 .UNSPECIFIED.);
#265=B_SPLINE_CURVE_WITH_KNOTS('',3,(#4620,#4621,#4622,#4623,#4624,#4625,
#4626,#4627,#4628,#4629,#4630,#4631,#4632,#4633,#4634,#4635,#4636,#4637,
#4638,#4639),.UNSPECIFIED.,.F.,.F.,(4,2,2,2,2,2,2,2,2,4),(0.140389663816901,
0.211667950083817,0.31749389924238,0.423319848400942,0.529145797559504,
0.634971746718067,0.740805721759975,0.846639696801883,0.952473671843791,
0.987029360618755),.UNSPECIFIED.);
#266=B_SPLINE_CURVE_WITH_KNOTS('',3,(#4640,#4641,#4642,#4643,#4644,#4645,
#4646,#4647,#4648,#4649,#4650,#4651,#4652,#4653,#4654,#4655,#4656,#4657,
#4658,#4659,#4660),.UNSPECIFIED.,.F.,.F.,(4,2,2,2,2,2,2,3,2,4),(0.987029360618755,
1.0583076468857,1.16413359604426,1.26995954520283,1.37578549436139,1.48161144351995,
1.58744541856186,1.69327939360377,1.79911336864568,1.83366905742067),
 .UNSPECIFIED.);
#267=B_SPLINE_CURVE_WITH_KNOTS('',3,(#4687,#4688,#4689,#4690,#4691,#4692,
#4693,#4694,#4695,#4696,#4697,#4698,#4699,#4700,#4701,#4702,#4703,#4704),
 .UNSPECIFIED.,.F.,.F.,(4,2,2,2,2,2,2,2,4),(-2.42440986895005,-2.27286833474305,
-2.12132680053606,-1.96981710112429,-1.81830740171253,-1.66679770230077,
-1.51528800288901,-1.36374646868202,-1.21220493447502),.UNSPECIFIED.);
#268=B_SPLINE_CURVE_WITH_KNOTS('',3,(#4716,#4717,#4718,#4719,#4720,#4721,
#4722,#4723,#4724,#4725,#4726,#4727,#4728,#4729,#4730,#4731,#4732,#4733),
 .UNSPECIFIED.,.F.,.F.,(4,2,2,2,2,2,2,2,4),(-2.42440986895003,-2.27286833474304,
-2.12132680053605,-1.96981710112428,-1.81830740171252,-1.66679770230076,
-1.515288002889,-1.36374646868201,-1.21220493447502),.UNSPECIFIED.);
#269=B_SPLINE_CURVE_WITH_KNOTS('',3,(#4883,#4884,#4885,#4886,#4887,#4888,
#4889,#4890,#4891,#4892,#4893,#4894,#4895,#4896,#4897,#4898,#4899,#4900,
#4901,#4902,#4903,#4904,#4905,#4906,#4907,#4908,#4909,#4910),
 .UNSPECIFIED.,.F.,.F.,(4,2,2,2,2,2,2,2,2,2,2,2,2,4),(-1.08391055751389,
-1.04041495858034,-0.976127049627852,-0.875975346180159,-0.713802892781725,
-0.606446034139209,-0.5422685089836,-0.478121096415875,-0.370996668444261,
-0.213675448646841,-0.11261366027741,-0.0448303332672381,-0.0212473968071398,
0.),.UNSPECIFIED.);
#270=B_SPLINE_CURVE_WITH_KNOTS('',3,(#4946,#4947,#4948,#4949,#4950,#4951,
#4952,#4953,#4954,#4955,#4956,#4957,#4958,#4959,#4960,#4961,#4962,#4963,
#4964,#4965,#4966,#4967,#4968,#4969,#4970,#4971,#4972,#4973),
 .UNSPECIFIED.,.F.,.F.,(4,2,2,2,2,2,2,2,2,2,2,2,2,4),(-1.08391055750046,
-1.04041495856732,-0.976127049615459,-0.875975346168904,-0.713802892772233,
-0.606446034130957,-0.542268508976211,-0.478121096409307,-0.370996668439296,
-0.213675448644088,-0.112613660276149,-0.0448303332669679,-0.0212473968071859,
0.),.UNSPECIFIED.);
#271=B_SPLINE_CURVE_WITH_KNOTS('',3,(#5009,#5010,#5011,#5012,#5013,#5014,
#5015,#5016,#5017,#5018,#5019,#5020,#5021,#5022,#5023,#5024,#5025,#5026,
#5027,#5028,#5029,#5030,#5031,#5032,#5033,#5034,#5035,#5036),
 .UNSPECIFIED.,.F.,.F.,(4,2,2,2,2,2,2,2,2,2,2,2,2,4),(-1.0839105575165,
-1.04041495858262,-0.976127049629671,-0.8759753461813,-0.713802892781876,
-0.606446034138857,-0.542268508983049,-0.478121096415206,-0.370996668443923,
-0.21367544864674,-0.112613660277534,-0.0448303332674202,-0.021247396807171,
0.),.UNSPECIFIED.);
#272=FACE_OUTER_BOUND('',#412,.T.);
#273=FACE_OUTER_BOUND('',#413,.T.);
#274=FACE_OUTER_BOUND('',#414,.T.);
#275=FACE_OUTER_BOUND('',#415,.T.);
#276=FACE_OUTER_BOUND('',#416,.T.);
#277=FACE_OUTER_BOUND('',#417,.T.);
#278=FACE_OUTER_BOUND('',#418,.T.);
#279=FACE_OUTER_BOUND('',#419,.T.);
#280=FACE_OUTER_BOUND('',#420,.T.);
#281=FACE_OUTER_BOUND('',#421,.T.);
#282=FACE_OUTER_BOUND('',#422,.T.);
#283=FACE_OUTER_BOUND('',#423,.T.);
#284=FACE_OUTER_BOUND('',#424,.T.);
#285=FACE_OUTER_BOUND('',#425,.T.);
#286=FACE_OUTER_BOUND('',#426,.T.);
#287=FACE_OUTER_BOUND('',#427,.T.);
#288=FACE_OUTER_BOUND('',#428,.T.);
#289=FACE_OUTER_BOUND('',#429,.T.);
#290=FACE_OUTER_BOUND('',#430,.T.);
#291=FACE_OUTER_BOUND('',#432,.T.);
#292=FACE_OUTER_BOUND('',#434,.T.);
#293=FACE_OUTER_BOUND('',#435,.T.);
#294=FACE_OUTER_BOUND('',#437,.T.);
#295=FACE_OUTER_BOUND('',#438,.T.);
#296=FACE_OUTER_BOUND('',#440,.T.);
#297=FACE_OUTER_BOUND('',#441,.T.);
#298=FACE_OUTER_BOUND('',#443,.T.);
#299=FACE_OUTER_BOUND('',#444,.T.);
#300=FACE_OUTER_BOUND('',#446,.T.);
#301=FACE_OUTER_BOUND('',#447,.T.);
#302=FACE_OUTER_BOUND('',#449,.T.);
#303=FACE_OUTER_BOUND('',#450,.T.);
#304=FACE_OUTER_BOUND('',#452,.T.);
#305=FACE_OUTER_BOUND('',#453,.T.);
#306=FACE_OUTER_BOUND('',#455,.T.);
#307=FACE_OUTER_BOUND('',#456,.T.);
#308=FACE_OUTER_BOUND('',#458,.T.);
#309=FACE_OUTER_BOUND('',#459,.T.);
#310=FACE_OUTER_BOUND('',#472,.T.);
#311=FACE_OUTER_BOUND('',#473,.T.);
#312=FACE_OUTER_BOUND('',#475,.T.);
#313=FACE_OUTER_BOUND('',#476,.T.);
#314=FACE_OUTER_BOUND('',#477,.T.);
#315=FACE_OUTER_BOUND('',#478,.T.);
#316=FACE_OUTER_BOUND('',#479,.T.);
#317=FACE_OUTER_BOUND('',#480,.T.);
#318=FACE_OUTER_BOUND('',#482,.T.);
#319=FACE_OUTER_BOUND('',#483,.T.);
#320=FACE_OUTER_BOUND('',#485,.T.);
#321=FACE_OUTER_BOUND('',#486,.T.);
#322=FACE_OUTER_BOUND('',#488,.T.);
#323=FACE_OUTER_BOUND('',#489,.T.);
#324=FACE_OUTER_BOUND('',#491,.T.);
#325=FACE_OUTER_BOUND('',#492,.T.);
#326=FACE_OUTER_BOUND('',#494,.T.);
#327=FACE_OUTER_BOUND('',#495,.T.);
#328=FACE_OUTER_BOUND('',#497,.T.);
#329=FACE_OUTER_BOUND('',#498,.T.);
#330=FACE_OUTER_BOUND('',#500,.T.);
#331=FACE_OUTER_BOUND('',#501,.T.);
#332=FACE_OUTER_BOUND('',#503,.T.);
#333=FACE_OUTER_BOUND('',#504,.T.);
#334=FACE_OUTER_BOUND('',#505,.T.);
#335=FACE_OUTER_BOUND('',#506,.T.);
#336=FACE_OUTER_BOUND('',#507,.T.);
#337=FACE_OUTER_BOUND('',#508,.T.);
#338=FACE_OUTER_BOUND('',#509,.T.);
#339=FACE_OUTER_BOUND('',#510,.T.);
#340=FACE_OUTER_BOUND('',#511,.T.);
#341=FACE_OUTER_BOUND('',#512,.T.);
#342=FACE_OUTER_BOUND('',#514,.T.);
#343=FACE_OUTER_BOUND('',#515,.T.);
#344=FACE_OUTER_BOUND('',#517,.T.);
#345=FACE_OUTER_BOUND('',#518,.T.);
#346=FACE_OUTER_BOUND('',#520,.T.);
#347=FACE_OUTER_BOUND('',#521,.T.);
#348=FACE_OUTER_BOUND('',#523,.T.);
#349=FACE_OUTER_BOUND('',#524,.T.);
#350=FACE_OUTER_BOUND('',#526,.T.);
#351=FACE_OUTER_BOUND('',#527,.T.);
#352=FACE_OUTER_BOUND('',#529,.T.);
#353=FACE_OUTER_BOUND('',#530,.T.);
#354=FACE_OUTER_BOUND('',#532,.T.);
#355=FACE_OUTER_BOUND('',#533,.T.);
#356=FACE_OUTER_BOUND('',#535,.T.);
#357=FACE_OUTER_BOUND('',#536,.T.);
#358=FACE_OUTER_BOUND('',#537,.T.);
#359=FACE_OUTER_BOUND('',#538,.T.);
#360=FACE_OUTER_BOUND('',#539,.T.);
#361=FACE_OUTER_BOUND('',#540,.T.);
#362=FACE_OUTER_BOUND('',#541,.T.);
#363=FACE_OUTER_BOUND('',#543,.T.);
#364=FACE_OUTER_BOUND('',#544,.T.);
#365=FACE_OUTER_BOUND('',#545,.T.);
#366=FACE_OUTER_BOUND('',#546,.T.);
#367=FACE_OUTER_BOUND('',#547,.T.);
#368=FACE_OUTER_BOUND('',#548,.T.);
#369=FACE_OUTER_BOUND('',#550,.T.);
#370=FACE_OUTER_BOUND('',#551,.T.);
#371=FACE_OUTER_BOUND('',#552,.T.);
#372=FACE_OUTER_BOUND('',#553,.T.);
#373=FACE_OUTER_BOUND('',#554,.T.);
#374=FACE_OUTER_BOUND('',#555,.T.);
#375=FACE_OUTER_BOUND('',#557,.T.);
#376=FACE_OUTER_BOUND('',#558,.T.);
#377=FACE_OUTER_BOUND('',#559,.T.);
#378=FACE_OUTER_BOUND('',#560,.T.);
#379=FACE_OUTER_BOUND('',#561,.T.);
#380=FACE_OUTER_BOUND('',#562,.T.);
#381=FACE_OUTER_BOUND('',#563,.T.);
#382=FACE_OUTER_BOUND('',#564,.T.);
#383=FACE_OUTER_BOUND('',#565,.T.);
#384=FACE_OUTER_BOUND('',#566,.T.);
#385=FACE_OUTER_BOUND('',#567,.T.);
#386=FACE_OUTER_BOUND('',#569,.T.);
#387=FACE_OUTER_BOUND('',#571,.T.);
#388=FACE_OUTER_BOUND('',#572,.T.);
#389=FACE_OUTER_BOUND('',#573,.T.);
#390=FACE_OUTER_BOUND('',#575,.T.);
#391=FACE_OUTER_BOUND('',#576,.T.);
#392=FACE_OUTER_BOUND('',#577,.T.);
#393=FACE_OUTER_BOUND('',#579,.T.);
#394=FACE_OUTER_BOUND('',#581,.T.);
#395=FACE_OUTER_BOUND('',#582,.T.);
#396=FACE_OUTER_BOUND('',#583,.T.);
#397=FACE_OUTER_BOUND('',#585,.T.);
#398=FACE_OUTER_BOUND('',#586,.T.);
#399=FACE_OUTER_BOUND('',#587,.T.);
#400=FACE_OUTER_BOUND('',#589,.T.);
#401=FACE_OUTER_BOUND('',#591,.T.);
#402=FACE_OUTER_BOUND('',#592,.T.);
#403=FACE_OUTER_BOUND('',#593,.T.);
#404=FACE_OUTER_BOUND('',#595,.T.);
#405=FACE_OUTER_BOUND('',#596,.T.);
#406=FACE_OUTER_BOUND('',#597,.T.);
#407=FACE_OUTER_BOUND('',#599,.T.);
#408=FACE_OUTER_BOUND('',#601,.T.);
#409=FACE_OUTER_BOUND('',#602,.T.);
#410=FACE_OUTER_BOUND('',#603,.T.);
#411=FACE_OUTER_BOUND('',#605,.T.);
#412=EDGE_LOOP('',(#1524,#1525,#1526,#1527));
#413=EDGE_LOOP('',(#1528,#1529,#1530,#1531));
#414=EDGE_LOOP('',(#1532,#1533,#1534,#1535));
#415=EDGE_LOOP('',(#1536,#1537,#1538,#1539,#1540,#1541));
#416=EDGE_LOOP('',(#1542,#1543,#1544,#1545,#1546));
#417=EDGE_LOOP('',(#1547,#1548,#1549,#1550,#1551));
#418=EDGE_LOOP('',(#1552,#1553,#1554,#1555));
#419=EDGE_LOOP('',(#1556,#1557,#1558,#1559));
#420=EDGE_LOOP('',(#1560,#1561,#1562,#1563,#1564,#1565));
#421=EDGE_LOOP('',(#1566,#1567,#1568,#1569,#1570));
#422=EDGE_LOOP('',(#1571,#1572,#1573,#1574,#1575));
#423=EDGE_LOOP('',(#1576,#1577,#1578,#1579));
#424=EDGE_LOOP('',(#1580,#1581,#1582,#1583,#1584,#1585));
#425=EDGE_LOOP('',(#1586,#1587,#1588,#1589,#1590));
#426=EDGE_LOOP('',(#1591,#1592,#1593,#1594,#1595));
#427=EDGE_LOOP('',(#1596,#1597,#1598,#1599));
#428=EDGE_LOOP('',(#1600,#1601,#1602,#1603));
#429=EDGE_LOOP('',(#1604,#1605,#1606,#1607));
#430=EDGE_LOOP('',(#1608));
#431=EDGE_LOOP('',(#1609,#1610,#1611,#1612,#1613,#1614,#1615,#1616,#1617,
#1618,#1619,#1620));
#432=EDGE_LOOP('',(#1621));
#433=EDGE_LOOP('',(#1622,#1623,#1624,#1625,#1626,#1627,#1628,#1629,#1630,
#1631,#1632,#1633));
#434=EDGE_LOOP('',(#1634,#1635,#1636,#1637));
#435=EDGE_LOOP('',(#1638,#1639,#1640,#1641,#1642,#1643,#1644,#1645,#1646,
#1647,#1648,#1649));
#436=EDGE_LOOP('',(#1650));
#437=EDGE_LOOP('',(#1651,#1652,#1653,#1654,#1655,#1656,#1657,#1658,#1659,
#1660,#1661,#1662));
#438=EDGE_LOOP('',(#1663));
#439=EDGE_LOOP('',(#1664));
#440=EDGE_LOOP('',(#1665,#1666,#1667,#1668,#1669,#1670,#1671,#1672));
#441=EDGE_LOOP('',(#1673));
#442=EDGE_LOOP('',(#1674));
#443=EDGE_LOOP('',(#1675,#1676,#1677,#1678,#1679,#1680));
#444=EDGE_LOOP('',(#1681));
#445=EDGE_LOOP('',(#1682));
#446=EDGE_LOOP('',(#1683,#1684,#1685,#1686,#1687,#1688));
#447=EDGE_LOOP('',(#1689));
#448=EDGE_LOOP('',(#1690));
#449=EDGE_LOOP('',(#1691,#1692,#1693,#1694,#1695,#1696));
#450=EDGE_LOOP('',(#1697));
#451=EDGE_LOOP('',(#1698));
#452=EDGE_LOOP('',(#1699,#1700,#1701,#1702));
#453=EDGE_LOOP('',(#1703));
#454=EDGE_LOOP('',(#1704));
#455=EDGE_LOOP('',(#1705,#1706,#1707,#1708));
#456=EDGE_LOOP('',(#1709));
#457=EDGE_LOOP('',(#1710));
#458=EDGE_LOOP('',(#1711,#1712,#1713,#1714));
#459=EDGE_LOOP('',(#1715,#1716,#1717,#1718));
#460=EDGE_LOOP('',(#1719,#1720));
#461=EDGE_LOOP('',(#1721,#1722));
#462=EDGE_LOOP('',(#1723,#1724));
#463=EDGE_LOOP('',(#1725,#1726));
#464=EDGE_LOOP('',(#1727,#1728));
#465=EDGE_LOOP('',(#1729,#1730));
#466=EDGE_LOOP('',(#1731,#1732));
#467=EDGE_LOOP('',(#1733,#1734));
#468=EDGE_LOOP('',(#1735,#1736));
#469=EDGE_LOOP('',(#1737,#1738));
#470=EDGE_LOOP('',(#1739,#1740));
#471=EDGE_LOOP('',(#1741,#1742));
#472=EDGE_LOOP('',(#1743));
#473=EDGE_LOOP('',(#1744));
#474=EDGE_LOOP('',(#1745));
#475=EDGE_LOOP('',(#1746,#1747,#1748,#1749));
#476=EDGE_LOOP('',(#1750,#1751,#1752,#1753,#1754));
#477=EDGE_LOOP('',(#1755,#1756,#1757,#1758,#1759));
#478=EDGE_LOOP('',(#1760,#1761,#1762,#1763,#1764));
#479=EDGE_LOOP('',(#1765,#1766,#1767,#1768,#1769));
#480=EDGE_LOOP('',(#1770));
#481=EDGE_LOOP('',(#1771));
#482=EDGE_LOOP('',(#1772,#1773,#1774,#1775,#1776,#1777,#1778,#1779));
#483=EDGE_LOOP('',(#1780));
#484=EDGE_LOOP('',(#1781));
#485=EDGE_LOOP('',(#1782,#1783,#1784,#1785,#1786,#1787,#1788,#1789));
#486=EDGE_LOOP('',(#1790));
#487=EDGE_LOOP('',(#1791));
#488=EDGE_LOOP('',(#1792,#1793,#1794,#1795,#1796,#1797));
#489=EDGE_LOOP('',(#1798));
#490=EDGE_LOOP('',(#1799));
#491=EDGE_LOOP('',(#1800,#1801,#1802,#1803,#1804,#1805));
#492=EDGE_LOOP('',(#1806));
#493=EDGE_LOOP('',(#1807));
#494=EDGE_LOOP('',(#1808,#1809,#1810,#1811,#1812,#1813));
#495=EDGE_LOOP('',(#1814));
#496=EDGE_LOOP('',(#1815));
#497=EDGE_LOOP('',(#1816,#1817,#1818,#1819,#1820,#1821));
#498=EDGE_LOOP('',(#1822));
#499=EDGE_LOOP('',(#1823));
#500=EDGE_LOOP('',(#1824,#1825,#1826,#1827,#1828,#1829));
#501=EDGE_LOOP('',(#1830));
#502=EDGE_LOOP('',(#1831));
#503=EDGE_LOOP('',(#1832,#1833,#1834,#1835,#1836,#1837));
#504=EDGE_LOOP('',(#1838,#1839,#1840,#1841,#1842));
#505=EDGE_LOOP('',(#1843,#1844,#1845,#1846,#1847));
#506=EDGE_LOOP('',(#1848,#1849,#1850,#1851,#1852));
#507=EDGE_LOOP('',(#1853,#1854,#1855,#1856,#1857));
#508=EDGE_LOOP('',(#1858,#1859,#1860,#1861,#1862));
#509=EDGE_LOOP('',(#1863,#1864,#1865,#1866,#1867));
#510=EDGE_LOOP('',(#1868,#1869,#1870,#1871,#1872));
#511=EDGE_LOOP('',(#1873,#1874,#1875,#1876,#1877));
#512=EDGE_LOOP('',(#1878));
#513=EDGE_LOOP('',(#1879));
#514=EDGE_LOOP('',(#1880,#1881,#1882,#1883));
#515=EDGE_LOOP('',(#1884));
#516=EDGE_LOOP('',(#1885));
#517=EDGE_LOOP('',(#1886,#1887,#1888,#1889));
#518=EDGE_LOOP('',(#1890));
#519=EDGE_LOOP('',(#1891));
#520=EDGE_LOOP('',(#1892,#1893,#1894,#1895));
#521=EDGE_LOOP('',(#1896));
#522=EDGE_LOOP('',(#1897));
#523=EDGE_LOOP('',(#1898,#1899,#1900,#1901));
#524=EDGE_LOOP('',(#1902));
#525=EDGE_LOOP('',(#1903));
#526=EDGE_LOOP('',(#1904,#1905,#1906,#1907));
#527=EDGE_LOOP('',(#1908));
#528=EDGE_LOOP('',(#1909));
#529=EDGE_LOOP('',(#1910,#1911,#1912,#1913));
#530=EDGE_LOOP('',(#1914));
#531=EDGE_LOOP('',(#1915));
#532=EDGE_LOOP('',(#1916,#1917,#1918,#1919));
#533=EDGE_LOOP('',(#1920));
#534=EDGE_LOOP('',(#1921));
#535=EDGE_LOOP('',(#1922,#1923,#1924,#1925));
#536=EDGE_LOOP('',(#1926,#1927,#1928,#1929));
#537=EDGE_LOOP('',(#1930,#1931,#1932,#1933));
#538=EDGE_LOOP('',(#1934,#1935,#1936,#1937,#1938,#1939,#1940));
#539=EDGE_LOOP('',(#1941,#1942,#1943,#1944,#1945,#1946,#1947));
#540=EDGE_LOOP('',(#1948,#1949,#1950,#1951));
#541=EDGE_LOOP('',(#1952,#1953,#1954,#1955));
#542=EDGE_LOOP('',(#1956,#1957,#1958,#1959));
#543=EDGE_LOOP('',(#1960,#1961,#1962,#1963));
#544=EDGE_LOOP('',(#1964,#1965,#1966,#1967));
#545=EDGE_LOOP('',(#1968,#1969,#1970,#1971,#1972,#1973,#1974));
#546=EDGE_LOOP('',(#1975,#1976,#1977,#1978,#1979,#1980,#1981));
#547=EDGE_LOOP('',(#1982,#1983,#1984,#1985));
#548=EDGE_LOOP('',(#1986,#1987,#1988,#1989));
#549=EDGE_LOOP('',(#1990,#1991,#1992,#1993));
#550=EDGE_LOOP('',(#1994,#1995,#1996,#1997));
#551=EDGE_LOOP('',(#1998,#1999,#2000,#2001));
#552=EDGE_LOOP('',(#2002,#2003,#2004,#2005,#2006,#2007,#2008));
#553=EDGE_LOOP('',(#2009,#2010,#2011,#2012,#2013,#2014,#2015));
#554=EDGE_LOOP('',(#2016,#2017,#2018,#2019));
#555=EDGE_LOOP('',(#2020,#2021,#2022,#2023));
#556=EDGE_LOOP('',(#2024,#2025,#2026,#2027));
#557=EDGE_LOOP('',(#2028,#2029,#2030,#2031));
#558=EDGE_LOOP('',(#2032,#2033,#2034,#2035));
#559=EDGE_LOOP('',(#2036,#2037,#2038,#2039));
#560=EDGE_LOOP('',(#2040,#2041,#2042,#2043));
#561=EDGE_LOOP('',(#2044,#2045,#2046,#2047));
#562=EDGE_LOOP('',(#2048,#2049,#2050,#2051));
#563=EDGE_LOOP('',(#2052,#2053,#2054,#2055));
#564=EDGE_LOOP('',(#2056,#2057,#2058,#2059));
#565=EDGE_LOOP('',(#2060,#2061,#2062,#2063));
#566=EDGE_LOOP('',(#2064,#2065,#2066,#2067));
#567=EDGE_LOOP('',(#2068));
#568=EDGE_LOOP('',(#2069));
#569=EDGE_LOOP('',(#2070));
#570=EDGE_LOOP('',(#2071));
#571=EDGE_LOOP('',(#2072,#2073,#2074,#2075));
#572=EDGE_LOOP('',(#2076,#2077,#2078,#2079));
#573=EDGE_LOOP('',(#2080));
#574=EDGE_LOOP('',(#2081));
#575=EDGE_LOOP('',(#2082,#2083,#2084,#2085));
#576=EDGE_LOOP('',(#2086,#2087,#2088,#2089));
#577=EDGE_LOOP('',(#2090));
#578=EDGE_LOOP('',(#2091));
#579=EDGE_LOOP('',(#2092));
#580=EDGE_LOOP('',(#2093));
#581=EDGE_LOOP('',(#2094,#2095,#2096,#2097));
#582=EDGE_LOOP('',(#2098,#2099,#2100,#2101));
#583=EDGE_LOOP('',(#2102));
#584=EDGE_LOOP('',(#2103));
#585=EDGE_LOOP('',(#2104,#2105,#2106,#2107));
#586=EDGE_LOOP('',(#2108,#2109,#2110,#2111));
#587=EDGE_LOOP('',(#2112));
#588=EDGE_LOOP('',(#2113));
#589=EDGE_LOOP('',(#2114));
#590=EDGE_LOOP('',(#2115));
#591=EDGE_LOOP('',(#2116,#2117,#2118,#2119));
#592=EDGE_LOOP('',(#2120,#2121,#2122,#2123));
#593=EDGE_LOOP('',(#2124));
#594=EDGE_LOOP('',(#2125));
#595=EDGE_LOOP('',(#2126,#2127,#2128,#2129));
#596=EDGE_LOOP('',(#2130,#2131,#2132,#2133));
#597=EDGE_LOOP('',(#2134));
#598=EDGE_LOOP('',(#2135));
#599=EDGE_LOOP('',(#2136));
#600=EDGE_LOOP('',(#2137));
#601=EDGE_LOOP('',(#2138,#2139,#2140,#2141));
#602=EDGE_LOOP('',(#2142,#2143,#2144,#2145));
#603=EDGE_LOOP('',(#2146));
#604=EDGE_LOOP('',(#2147));
#605=EDGE_LOOP('',(#2148,#2149,#2150,#2151));
#606=CIRCLE('',#2427,15.);
#607=CIRCLE('',#2428,15.);
#608=CIRCLE('',#2430,15.);
#609=CIRCLE('',#2431,15.);
#610=CIRCLE('',#2433,15.);
#611=CIRCLE('',#2434,15.);
#612=CIRCLE('',#2440,15.);
#613=CIRCLE('',#2441,15.);
#614=CIRCLE('',#2451,15.);
#615=CIRCLE('',#2452,15.);
#616=CIRCLE('',#2454,15.);
#617=CIRCLE('',#2455,15.);
#618=CIRCLE('',#2457,17.);
#619=CIRCLE('',#2458,14.5);
#620=CIRCLE('',#2459,14.5);
#621=CIRCLE('',#2460,14.5);
#622=CIRCLE('',#2462,17.);
#623=CIRCLE('',#2465,12.9999999999984);
#624=CIRCLE('',#2467,14.5);
#625=CIRCLE('',#2468,14.5);
#626=CIRCLE('',#2469,14.5);
#627=CIRCLE('',#2471,4.00000000000012);
#628=CIRCLE('',#2472,3.50000000000012);
#629=CIRCLE('',#2475,4.00000000000001);
#630=CIRCLE('',#2476,3.5);
#631=CIRCLE('',#2479,4.00000000000001);
#632=CIRCLE('',#2480,3.49999999999992);
#633=CIRCLE('',#2483,4.);
#634=CIRCLE('',#2484,3.49999999999998);
#635=CIRCLE('',#2487,3.50000000000012);
#636=CIRCLE('',#2488,2.80000000000012);
#637=CIRCLE('',#2491,3.5);
#638=CIRCLE('',#2492,2.79999999999998);
#639=CIRCLE('',#2495,3.49999999999992);
#640=CIRCLE('',#2496,2.79999999999991);
#641=CIRCLE('',#2499,12.9999999999984);
#642=CIRCLE('',#2502,3.49999999999998);
#643=CIRCLE('',#2503,2.79999999999999);
#644=CIRCLE('',#2510,4.00000000000012);
#645=CIRCLE('',#2511,3.50000000000012);
#646=CIRCLE('',#2514,4.00000000000012);
#647=CIRCLE('',#2515,3.50000000000012);
#648=CIRCLE('',#2518,4.00000000000001);
#649=CIRCLE('',#2519,3.5);
#650=CIRCLE('',#2522,4.00000000000001);
#651=CIRCLE('',#2523,3.5);
#652=CIRCLE('',#2526,4.00000000000001);
#653=CIRCLE('',#2527,3.49999999999992);
#654=CIRCLE('',#2530,4.00000000000001);
#655=CIRCLE('',#2531,3.49999999999992);
#656=CIRCLE('',#2534,4.);
#657=CIRCLE('',#2535,3.49999999999998);
#658=CIRCLE('',#2538,4.);
#659=CIRCLE('',#2539,3.49999999999998);
#660=CIRCLE('',#2542,2.80000000000012);
#661=CIRCLE('',#2544,2.80000000000012);
#662=CIRCLE('',#2546,2.79999999999998);
#663=CIRCLE('',#2548,2.79999999999998);
#664=CIRCLE('',#2550,2.79999999999991);
#665=CIRCLE('',#2552,2.79999999999991);
#666=CIRCLE('',#2554,2.79999999999999);
#667=CIRCLE('',#2556,2.79999999999999);
#668=CIRCLE('',#2558,3.50000000000012);
#669=CIRCLE('',#2561,3.50000000000012);
#670=CIRCLE('',#2564,3.5);
#671=CIRCLE('',#2567,3.5);
#672=CIRCLE('',#2570,3.49999999999992);
#673=CIRCLE('',#2573,3.49999999999992);
#674=CIRCLE('',#2576,3.49999999999998);
#675=CIRCLE('',#2579,3.49999999999998);
#676=CIRCLE('',#2607,4.00000000000001);
#677=CIRCLE('',#2608,4.00000000000001);
#678=CIRCLE('',#2610,3.50000000000001);
#679=CIRCLE('',#2612,1.8);
#680=CIRCLE('',#2614,0.899999999999997);
#681=CIRCLE('',#2615,0.899999999999995);
#682=CIRCLE('',#2618,3.50000000000001);
#683=CIRCLE('',#2622,3.99999999999999);
#684=CIRCLE('',#2623,3.99999999999999);
#685=CIRCLE('',#2625,3.49999999999999);
#686=CIRCLE('',#2627,1.8);
#687=CIRCLE('',#2629,0.899999999999989);
#688=CIRCLE('',#2630,0.899999999999988);
#689=CIRCLE('',#2633,3.49999999999999);
#690=CIRCLE('',#2637,4.);
#691=CIRCLE('',#2638,4.);
#692=CIRCLE('',#2640,3.49999999999993);
#693=CIRCLE('',#2642,1.80000000000001);
#694=CIRCLE('',#2644,0.900000000000014);
#695=CIRCLE('',#2645,0.899999999999985);
#696=CIRCLE('',#2648,3.49999999999993);
#697=CIRCLE('',#2652,4.00000000000013);
#698=CIRCLE('',#2653,4.00000000000013);
#699=CIRCLE('',#2655,3.50000000000012);
#700=CIRCLE('',#2657,1.8);
#701=CIRCLE('',#2659,0.89999999999999);
#702=CIRCLE('',#2660,0.899999999999984);
#703=CIRCLE('',#2663,3.50000000000012);
#704=LINE('',#3341,#854);
#705=LINE('',#3345,#855);
#706=LINE('',#3350,#856);
#707=LINE('',#3354,#857);
#708=LINE('',#3361,#858);
#709=LINE('',#3364,#859);
#710=LINE('',#3368,#860);
#711=LINE('',#3394,#861);
#712=LINE('',#3420,#862);
#713=LINE('',#3445,#863);
#714=LINE('',#3466,#864);
#715=LINE('',#3491,#865);
#716=LINE('',#3512,#866);
#717=LINE('',#3536,#867);
#718=LINE('',#3568,#868);
#719=LINE('',#3571,#869);
#720=LINE('',#3575,#870);
#721=LINE('',#3601,#871);
#722=LINE('',#3627,#872);
#723=LINE('',#3652,#873);
#724=LINE('',#3673,#874);
#725=LINE('',#3698,#875);
#726=LINE('',#3719,#876);
#727=LINE('',#3743,#877);
#728=LINE('',#3773,#878);
#729=LINE('',#3799,#879);
#730=LINE('',#3825,#880);
#731=LINE('',#3850,#881);
#732=LINE('',#3871,#882);
#733=LINE('',#3896,#883);
#734=LINE('',#3917,#884);
#735=LINE('',#3941,#885);
#736=LINE('',#3973,#886);
#737=LINE('',#3976,#887);
#738=LINE('',#3980,#888);
#739=LINE('',#3984,#889);
#740=LINE('',#3990,#890);
#741=LINE('',#3993,#891);
#742=LINE('',#3995,#892);
#743=LINE('',#3998,#893);
#744=LINE('',#4000,#894);
#745=LINE('',#4003,#895);
#746=LINE('',#4008,#896);
#747=LINE('',#4010,#897);
#748=LINE('',#4011,#898);
#749=LINE('',#4013,#899);
#750=LINE('',#4015,#900);
#751=LINE('',#4016,#901);
#752=LINE('',#4018,#902);
#753=LINE('',#4020,#903);
#754=LINE('',#4021,#904);
#755=LINE('',#4023,#905);
#756=LINE('',#4026,#906);
#757=LINE('',#4028,#907);
#758=LINE('',#4029,#908);
#759=LINE('',#4031,#909);
#760=LINE('',#4033,#910);
#761=LINE('',#4034,#911);
#762=LINE('',#4036,#912);
#763=LINE('',#4038,#913);
#764=LINE('',#4039,#914);
#765=LINE('',#4044,#915);
#766=LINE('',#4047,#916);
#767=LINE('',#4049,#917);
#768=LINE('',#4052,#918);
#769=LINE('',#4054,#919);
#770=LINE('',#4057,#920);
#771=LINE('',#4064,#921);
#772=LINE('',#4066,#922);
#773=LINE('',#4086,#923);
#774=LINE('',#4093,#924);
#775=LINE('',#4100,#925);
#776=LINE('',#4107,#926);
#777=LINE('',#4114,#927);
#778=LINE('',#4121,#928);
#779=LINE('',#4128,#929);
#780=LINE('',#4132,#930);
#781=LINE('',#4668,#931);
#782=LINE('',#4670,#932);
#783=LINE('',#4672,#933);
#784=LINE('',#4674,#934);
#785=LINE('',#4676,#935);
#786=LINE('',#4683,#936);
#787=LINE('',#4685,#937);
#788=LINE('',#4705,#938);
#789=LINE('',#4712,#939);
#790=LINE('',#4714,#940);
#791=LINE('',#4734,#941);
#792=LINE('',#4741,#942);
#793=LINE('',#4748,#943);
#794=LINE('',#4755,#944);
#795=LINE('',#4762,#945);
#796=LINE('',#4769,#946);
#797=LINE('',#4776,#947);
#798=LINE('',#4779,#948);
#799=LINE('',#4783,#949);
#800=LINE('',#4787,#950);
#801=LINE('',#4791,#951);
#802=LINE('',#4795,#952);
#803=LINE('',#4799,#953);
#804=LINE('',#4803,#954);
#805=LINE('',#4807,#955);
#806=LINE('',#4813,#956);
#807=LINE('',#4818,#957);
#808=LINE('',#4823,#958);
#809=LINE('',#4828,#959);
#810=LINE('',#4833,#960);
#811=LINE('',#4838,#961);
#812=LINE('',#4843,#962);
#813=LINE('',#4848,#963);
#814=LINE('',#4850,#964);
#815=LINE('',#4852,#965);
#816=LINE('',#4855,#966);
#817=LINE('',#4856,#967);
#818=LINE('',#4859,#968);
#819=LINE('',#4860,#969);
#820=LINE('',#4913,#970);
#821=LINE('',#4915,#971);
#822=LINE('',#4918,#972);
#823=LINE('',#4919,#973);
#824=LINE('',#4922,#974);
#825=LINE('',#4923,#975);
#826=LINE('',#4976,#976);
#827=LINE('',#4978,#977);
#828=LINE('',#4981,#978);
#829=LINE('',#4982,#979);
#830=LINE('',#4985,#980);
#831=LINE('',#4986,#981);
#832=LINE('',#5039,#982);
#833=LINE('',#5041,#983);
#834=LINE('',#5044,#984);
#835=LINE('',#5046,#985);
#836=LINE('',#5049,#986);
#837=LINE('',#5051,#987);
#838=LINE('',#5058,#988);
#839=LINE('',#5070,#989);
#840=LINE('',#5073,#990);
#841=LINE('',#5078,#991);
#842=LINE('',#5084,#992);
#843=LINE('',#5096,#993);
#844=LINE('',#5099,#994);
#845=LINE('',#5104,#995);
#846=LINE('',#5110,#996);
#847=LINE('',#5122,#997);
#848=LINE('',#5125,#998);
#849=LINE('',#5130,#999);
#850=LINE('',#5136,#1000);
#851=LINE('',#5148,#1001);
#852=LINE('',#5151,#1002);
#853=LINE('',#5156,#1003);
#854=VECTOR('',#2684,3.99999999999999);
#855=VECTOR('',#2687,3.99999999999998);
#856=VECTOR('',#2692,3.99999999999999);
#857=VECTOR('',#2695,3.99999999999996);
#858=VECTOR('',#2702,57.);
#859=VECTOR('',#2705,57.);
#860=VECTOR('',#2708,13.3544586520373);
#861=VECTOR('',#2709,13.3544586520371);
#862=VECTOR('',#2712,13.3319433271509);
#863=VECTOR('',#2713,13.3319433271509);
#864=VECTOR('',#2716,13.2704303156128);
#865=VECTOR('',#2717,13.2704303156126);
#866=VECTOR('',#2720,3.88631345570718);
#867=VECTOR('',#2721,3.88631345570666);
#868=VECTOR('',#2726,57.);
#869=VECTOR('',#2729,57.);
#870=VECTOR('',#2732,13.3544586520373);
#871=VECTOR('',#2733,13.3544586520371);
#872=VECTOR('',#2736,13.3319433271511);
#873=VECTOR('',#2737,13.3319433271509);
#874=VECTOR('',#2740,13.2704303156128);
#875=VECTOR('',#2741,13.2704303156126);
#876=VECTOR('',#2744,3.88631345570709);
#877=VECTOR('',#2745,3.88631345570659);
#878=VECTOR('',#2748,13.3544586520373);
#879=VECTOR('',#2749,13.3544586520371);
#880=VECTOR('',#2752,13.331943327151);
#881=VECTOR('',#2753,13.3319433271509);
#882=VECTOR('',#2756,13.2704303156128);
#883=VECTOR('',#2757,13.2704303156126);
#884=VECTOR('',#2760,3.88631345570711);
#885=VECTOR('',#2761,3.8863134557066);
#886=VECTOR('',#2766,57.);
#887=VECTOR('',#2769,57.);
#888=VECTOR('',#2772,3.99999999999998);
#889=VECTOR('',#2775,3.99999999999998);
#890=VECTOR('',#2782,0.561081020730737);
#891=VECTOR('',#2785,0.561081020730727);
#892=VECTOR('',#2786,0.561081020730758);
#893=VECTOR('',#2789,0.561081020730749);
#894=VECTOR('',#2790,0.561081020730754);
#895=VECTOR('',#2793,0.561081020730736);
#896=VECTOR('',#2798,0.999999999999974);
#897=VECTOR('',#2799,1.00000000000001);
#898=VECTOR('',#2800,0.999999999999884);
#899=VECTOR('',#2801,1.);
#900=VECTOR('',#2802,1.00000000000001);
#901=VECTOR('',#2803,0.999999999999921);
#902=VECTOR('',#2804,0.999999999999996);
#903=VECTOR('',#2805,0.999999999999991);
#904=VECTOR('',#2806,0.99999999999989);
#905=VECTOR('',#2809,17.);
#906=VECTOR('',#2812,0.999999999999894);
#907=VECTOR('',#2813,1.00000000000001);
#908=VECTOR('',#2814,0.999999999999984);
#909=VECTOR('',#2815,0.99999999999989);
#910=VECTOR('',#2816,0.999999999999991);
#911=VECTOR('',#2817,0.999999999999996);
#912=VECTOR('',#2818,0.999999999999925);
#913=VECTOR('',#2819,1.00000000000001);
#914=VECTOR('',#2820,1.00000000000002);
#915=VECTOR('',#2825,0.56108102073074);
#916=VECTOR('',#2828,0.561081020730741);
#917=VECTOR('',#2829,0.561081020730736);
#918=VECTOR('',#2832,0.561081020730754);
#919=VECTOR('',#2833,0.561081020730749);
#920=VECTOR('',#2836,0.561081020730719);
#921=VECTOR('',#2845,4.00000000000012);
#922=VECTOR('',#2846,0.519472430034522);
#923=VECTOR('',#2847,0.519472430034611);
#924=VECTOR('',#2856,4.00000000000001);
#925=VECTOR('',#2865,4.00000000000001);
#926=VECTOR('',#2874,4.);
#927=VECTOR('',#2883,3.50000000000012);
#928=VECTOR('',#2892,3.5);
#929=VECTOR('',#2901,3.49999999999992);
#930=VECTOR('',#2906,12.9999999999984);
#931=VECTOR('',#2917,3.49999999999998);
#932=VECTOR('',#2920,2.80000000000012);
#933=VECTOR('',#2923,2.79999999999998);
#934=VECTOR('',#2926,2.79999999999991);
#935=VECTOR('',#2929,2.79999999999999);
#936=VECTOR('',#2938,4.00000000000012);
#937=VECTOR('',#2939,0.519472430034534);
#938=VECTOR('',#2940,0.519472430034598);
#939=VECTOR('',#2949,4.00000000000012);
#940=VECTOR('',#2950,0.519472430034482);
#941=VECTOR('',#2951,0.519472430034555);
#942=VECTOR('',#2960,4.00000000000001);
#943=VECTOR('',#2969,4.00000000000001);
#944=VECTOR('',#2978,4.00000000000001);
#945=VECTOR('',#2987,4.00000000000001);
#946=VECTOR('',#2996,4.);
#947=VECTOR('',#3005,4.);
#948=VECTOR('',#3008,2.80000000000012);
#949=VECTOR('',#3013,2.80000000000012);
#950=VECTOR('',#3018,2.79999999999998);
#951=VECTOR('',#3023,2.79999999999998);
#952=VECTOR('',#3028,2.79999999999991);
#953=VECTOR('',#3033,2.79999999999991);
#954=VECTOR('',#3038,2.79999999999999);
#955=VECTOR('',#3043,2.79999999999999);
#956=VECTOR('',#3052,3.50000000000012);
#957=VECTOR('',#3059,3.50000000000012);
#958=VECTOR('',#3066,3.5);
#959=VECTOR('',#3073,3.5);
#960=VECTOR('',#3080,3.49999999999992);
#961=VECTOR('',#3087,3.49999999999992);
#962=VECTOR('',#3094,3.49999999999998);
#963=VECTOR('',#3101,3.49999999999998);
#964=VECTOR('',#3104,57.);
#965=VECTOR('',#3107,57.);
#966=VECTOR('',#3110,0.519472430034682);
#967=VECTOR('',#3111,43.8431457505075);
#968=VECTOR('',#3114,43.8431457505077);
#969=VECTOR('',#3115,0.519472430034611);
#970=VECTOR('',#3120,57.);
#971=VECTOR('',#3123,57.);
#972=VECTOR('',#3126,0.51947243003468);
#973=VECTOR('',#3127,43.8431457505077);
#974=VECTOR('',#3130,43.8431457505077);
#975=VECTOR('',#3131,0.519472430034606);
#976=VECTOR('',#3136,57.);
#977=VECTOR('',#3139,57.);
#978=VECTOR('',#3142,0.5194724300347);
#979=VECTOR('',#3143,43.8431457505077);
#980=VECTOR('',#3146,43.8431457505077);
#981=VECTOR('',#3147,0.519472430034622);
#982=VECTOR('',#3152,3.99999999999998);
#983=VECTOR('',#3155,3.99999999999998);
#984=VECTOR('',#3160,3.99999999999997);
#985=VECTOR('',#3163,4.);
#986=VECTOR('',#3168,3.99999999999998);
#987=VECTOR('',#3171,3.99999999999998);
#988=VECTOR('',#3180,4.00000000000001);
#989=VECTOR('',#3195,0.899999999999993);
#990=VECTOR('',#3200,1.8);
#991=VECTOR('',#3207,3.50000000000002);
#992=VECTOR('',#3214,3.99999999999999);
#993=VECTOR('',#3229,0.899999999999994);
#994=VECTOR('',#3234,1.8);
#995=VECTOR('',#3241,3.49999999999999);
#996=VECTOR('',#3248,4.);
#997=VECTOR('',#3263,0.899999999999989);
#998=VECTOR('',#3268,1.80000000000001);
#999=VECTOR('',#3275,3.49999999999992);
#1000=VECTOR('',#3282,4.00000000000013);
#1001=VECTOR('',#3297,0.899999999999984);
#1002=VECTOR('',#3302,1.8);
#1003=VECTOR('',#3309,3.50000000000012);
#1004=VERTEX_POINT('',#3339);
#1005=VERTEX_POINT('',#3340);
#1006=VERTEX_POINT('',#3342);
#1007=VERTEX_POINT('',#3344);
#1008=VERTEX_POINT('',#3348);
#1009=VERTEX_POINT('',#3349);
#1010=VERTEX_POINT('',#3351);
#1011=VERTEX_POINT('',#3353);
#1012=VERTEX_POINT('',#3357);
#1013=VERTEX_POINT('',#3358);
#1014=VERTEX_POINT('',#3360);
#1015=VERTEX_POINT('',#3362);
#1016=VERTEX_POINT('',#3366);
#1017=VERTEX_POINT('',#3367);
#1018=VERTEX_POINT('',#3369);
#1019=VERTEX_POINT('',#3378);
#1020=VERTEX_POINT('',#3393);
#1021=VERTEX_POINT('',#3395);
#1022=VERTEX_POINT('',#3419);
#1023=VERTEX_POINT('',#3421);
#1024=VERTEX_POINT('',#3430);
#1025=VERTEX_POINT('',#3465);
#1026=VERTEX_POINT('',#3467);
#1027=VERTEX_POINT('',#3478);
#1028=VERTEX_POINT('',#3511);
#1029=VERTEX_POINT('',#3535);
#1030=VERTEX_POINT('',#3564);
#1031=VERTEX_POINT('',#3565);
#1032=VERTEX_POINT('',#3567);
#1033=VERTEX_POINT('',#3569);
#1034=VERTEX_POINT('',#3573);
#1035=VERTEX_POINT('',#3574);
#1036=VERTEX_POINT('',#3576);
#1037=VERTEX_POINT('',#3585);
#1038=VERTEX_POINT('',#3600);
#1039=VERTEX_POINT('',#3602);
#1040=VERTEX_POINT('',#3626);
#1041=VERTEX_POINT('',#3628);
#1042=VERTEX_POINT('',#3637);
#1043=VERTEX_POINT('',#3672);
#1044=VERTEX_POINT('',#3674);
#1045=VERTEX_POINT('',#3683);
#1046=VERTEX_POINT('',#3718);
#1047=VERTEX_POINT('',#3742);
#1048=VERTEX_POINT('',#3771);
#1049=VERTEX_POINT('',#3772);
#1050=VERTEX_POINT('',#3774);
#1051=VERTEX_POINT('',#3783);
#1052=VERTEX_POINT('',#3798);
#1053=VERTEX_POINT('',#3800);
#1054=VERTEX_POINT('',#3824);
#1055=VERTEX_POINT('',#3826);
#1056=VERTEX_POINT('',#3835);
#1057=VERTEX_POINT('',#3870);
#1058=VERTEX_POINT('',#3872);
#1059=VERTEX_POINT('',#3883);
#1060=VERTEX_POINT('',#3916);
#1061=VERTEX_POINT('',#3940);
#1062=VERTEX_POINT('',#3969);
#1063=VERTEX_POINT('',#3970);
#1064=VERTEX_POINT('',#3972);
#1065=VERTEX_POINT('',#3974);
#1066=VERTEX_POINT('',#3978);
#1067=VERTEX_POINT('',#3979);
#1068=VERTEX_POINT('',#3981);
#1069=VERTEX_POINT('',#3983);
#1070=VERTEX_POINT('',#3987);
#1071=VERTEX_POINT('',#3989);
#1072=VERTEX_POINT('',#3991);
#1073=VERTEX_POINT('',#3994);
#1074=VERTEX_POINT('',#3996);
#1075=VERTEX_POINT('',#3999);
#1076=VERTEX_POINT('',#4001);
#1077=VERTEX_POINT('',#4005);
#1078=VERTEX_POINT('',#4007);
#1079=VERTEX_POINT('',#4009);
#1080=VERTEX_POINT('',#4012);
#1081=VERTEX_POINT('',#4014);
#1082=VERTEX_POINT('',#4017);
#1083=VERTEX_POINT('',#4019);
#1084=VERTEX_POINT('',#4025);
#1085=VERTEX_POINT('',#4027);
#1086=VERTEX_POINT('',#4030);
#1087=VERTEX_POINT('',#4032);
#1088=VERTEX_POINT('',#4035);
#1089=VERTEX_POINT('',#4037);
#1090=VERTEX_POINT('',#4040);
#1091=VERTEX_POINT('',#4043);
#1092=VERTEX_POINT('',#4045);
#1093=VERTEX_POINT('',#4048);
#1094=VERTEX_POINT('',#4050);
#1095=VERTEX_POINT('',#4053);
#1096=VERTEX_POINT('',#4055);
#1097=VERTEX_POINT('',#4059);
#1098=VERTEX_POINT('',#4061);
#1099=VERTEX_POINT('',#4065);
#1100=VERTEX_POINT('',#4067);
#1101=VERTEX_POINT('',#4088);
#1102=VERTEX_POINT('',#4090);
#1103=VERTEX_POINT('',#4095);
#1104=VERTEX_POINT('',#4097);
#1105=VERTEX_POINT('',#4102);
#1106=VERTEX_POINT('',#4104);
#1107=VERTEX_POINT('',#4109);
#1108=VERTEX_POINT('',#4111);
#1109=VERTEX_POINT('',#4116);
#1110=VERTEX_POINT('',#4118);
#1111=VERTEX_POINT('',#4123);
#1112=VERTEX_POINT('',#4125);
#1113=VERTEX_POINT('',#4130);
#1114=VERTEX_POINT('',#4133);
#1115=VERTEX_POINT('',#4134);
#1116=VERTEX_POINT('',#4180);
#1117=VERTEX_POINT('',#4181);
#1118=VERTEX_POINT('',#4227);
#1119=VERTEX_POINT('',#4228);
#1120=VERTEX_POINT('',#4270);
#1121=VERTEX_POINT('',#4271);
#1122=VERTEX_POINT('',#4313);
#1123=VERTEX_POINT('',#4314);
#1124=VERTEX_POINT('',#4356);
#1125=VERTEX_POINT('',#4357);
#1126=VERTEX_POINT('',#4399);
#1127=VERTEX_POINT('',#4400);
#1128=VERTEX_POINT('',#4442);
#1129=VERTEX_POINT('',#4443);
#1130=VERTEX_POINT('',#4485);
#1131=VERTEX_POINT('',#4486);
#1132=VERTEX_POINT('',#4532);
#1133=VERTEX_POINT('',#4533);
#1134=VERTEX_POINT('',#4575);
#1135=VERTEX_POINT('',#4576);
#1136=VERTEX_POINT('',#4618);
#1137=VERTEX_POINT('',#4619);
#1138=VERTEX_POINT('',#4663);
#1139=VERTEX_POINT('',#4665);
#1140=VERTEX_POINT('',#4678);
#1141=VERTEX_POINT('',#4680);
#1142=VERTEX_POINT('',#4684);
#1143=VERTEX_POINT('',#4686);
#1144=VERTEX_POINT('',#4707);
#1145=VERTEX_POINT('',#4709);
#1146=VERTEX_POINT('',#4713);
#1147=VERTEX_POINT('',#4715);
#1148=VERTEX_POINT('',#4736);
#1149=VERTEX_POINT('',#4738);
#1150=VERTEX_POINT('',#4743);
#1151=VERTEX_POINT('',#4745);
#1152=VERTEX_POINT('',#4750);
#1153=VERTEX_POINT('',#4752);
#1154=VERTEX_POINT('',#4757);
#1155=VERTEX_POINT('',#4759);
#1156=VERTEX_POINT('',#4764);
#1157=VERTEX_POINT('',#4766);
#1158=VERTEX_POINT('',#4771);
#1159=VERTEX_POINT('',#4773);
#1160=VERTEX_POINT('',#4778);
#1161=VERTEX_POINT('',#4782);
#1162=VERTEX_POINT('',#4786);
#1163=VERTEX_POINT('',#4790);
#1164=VERTEX_POINT('',#4794);
#1165=VERTEX_POINT('',#4798);
#1166=VERTEX_POINT('',#4802);
#1167=VERTEX_POINT('',#4806);
#1168=VERTEX_POINT('',#4810);
#1169=VERTEX_POINT('',#4815);
#1170=VERTEX_POINT('',#4820);
#1171=VERTEX_POINT('',#4825);
#1172=VERTEX_POINT('',#4830);
#1173=VERTEX_POINT('',#4835);
#1174=VERTEX_POINT('',#4840);
#1175=VERTEX_POINT('',#4845);
#1176=VERTEX_POINT('',#4854);
#1177=VERTEX_POINT('',#4858);
#1178=VERTEX_POINT('',#4917);
#1179=VERTEX_POINT('',#4921);
#1180=VERTEX_POINT('',#4980);
#1181=VERTEX_POINT('',#4984);
#1182=VERTEX_POINT('',#5055);
#1183=VERTEX_POINT('',#5057);
#1184=VERTEX_POINT('',#5061);
#1185=VERTEX_POINT('',#5064);
#1186=VERTEX_POINT('',#5067);
#1187=VERTEX_POINT('',#5069);
#1188=VERTEX_POINT('',#5075);
#1189=VERTEX_POINT('',#5081);
#1190=VERTEX_POINT('',#5083);
#1191=VERTEX_POINT('',#5087);
#1192=VERTEX_POINT('',#5090);
#1193=VERTEX_POINT('',#5093);
#1194=VERTEX_POINT('',#5095);
#1195=VERTEX_POINT('',#5101);
#1196=VERTEX_POINT('',#5107);
#1197=VERTEX_POINT('',#5109);
#1198=VERTEX_POINT('',#5113);
#1199=VERTEX_POINT('',#5116);
#1200=VERTEX_POINT('',#5119);
#1201=VERTEX_POINT('',#5121);
#1202=VERTEX_POINT('',#5127);
#1203=VERTEX_POINT('',#5133);
#1204=VERTEX_POINT('',#5135);
#1205=VERTEX_POINT('',#5139);
#1206=VERTEX_POINT('',#5142);
#1207=VERTEX_POINT('',#5145);
#1208=VERTEX_POINT('',#5147);
#1209=VERTEX_POINT('',#5153);
#1210=EDGE_CURVE('',#1004,#1005,#704,.F.);
#1211=EDGE_CURVE('',#1006,#1004,#606,.T.);
#1212=EDGE_CURVE('',#1007,#1006,#705,.T.);
#1213=EDGE_CURVE('',#1007,#1005,#607,.T.);
#1214=EDGE_CURVE('',#1008,#1009,#706,.T.);
#1215=EDGE_CURVE('',#1008,#1010,#608,.T.);
#1216=EDGE_CURVE('',#1011,#1010,#707,.F.);
#1217=EDGE_CURVE('',#1009,#1011,#609,.T.);
#1218=EDGE_CURVE('',#1012,#1013,#610,.T.);
#1219=EDGE_CURVE('',#1013,#1014,#708,.F.);
#1220=EDGE_CURVE('',#1015,#1014,#611,.T.);
#1221=EDGE_CURVE('',#1015,#1012,#709,.T.);
#1222=EDGE_CURVE('',#1016,#1017,#710,.T.);
#1223=EDGE_CURVE('',#1018,#1016,#206,.T.);
#1224=EDGE_CURVE('',#1019,#1018,#207,.T.);
#1225=EDGE_CURVE('',#1020,#1019,#711,.F.);
#1226=EDGE_CURVE('',#1021,#1020,#208,.T.);
#1227=EDGE_CURVE('',#1017,#1021,#209,.T.);
#1228=EDGE_CURVE('',#1022,#1016,#712,.T.);
#1229=EDGE_CURVE('',#1023,#1022,#210,.T.);
#1230=EDGE_CURVE('',#1024,#1023,#211,.T.);
#1231=EDGE_CURVE('',#1019,#1024,#713,.F.);
#1232=EDGE_CURVE('',#1016,#1019,#212,.T.);
#1233=EDGE_CURVE('',#1025,#1022,#714,.T.);
#1234=EDGE_CURVE('',#1026,#1025,#213,.T.);
#1235=EDGE_CURVE('',#1027,#1026,#214,.T.);
#1236=EDGE_CURVE('',#1024,#1027,#715,.F.);
#1237=EDGE_CURVE('',#1022,#1024,#215,.T.);
#1238=EDGE_CURVE('',#1027,#1028,#716,.F.);
#1239=EDGE_CURVE('',#1025,#1027,#216,.T.);
#1240=EDGE_CURVE('',#1029,#1025,#717,.T.);
#1241=EDGE_CURVE('',#1028,#1029,#217,.T.);
#1242=EDGE_CURVE('',#1030,#1031,#612,.T.);
#1243=EDGE_CURVE('',#1031,#1032,#718,.F.);
#1244=EDGE_CURVE('',#1033,#1032,#613,.T.);
#1245=EDGE_CURVE('',#1033,#1030,#719,.T.);
#1246=EDGE_CURVE('',#1034,#1035,#720,.T.);
#1247=EDGE_CURVE('',#1036,#1034,#218,.T.);
#1248=EDGE_CURVE('',#1037,#1036,#219,.T.);
#1249=EDGE_CURVE('',#1038,#1037,#721,.F.);
#1250=EDGE_CURVE('',#1039,#1038,#220,.T.);
#1251=EDGE_CURVE('',#1035,#1039,#221,.T.);
#1252=EDGE_CURVE('',#1040,#1034,#722,.T.);
#1253=EDGE_CURVE('',#1041,#1040,#222,.T.);
#1254=EDGE_CURVE('',#1042,#1041,#223,.T.);
#1255=EDGE_CURVE('',#1037,#1042,#723,.F.);
#1256=EDGE_CURVE('',#1034,#1037,#224,.T.);
#1257=EDGE_CURVE('',#1043,#1040,#724,.T.);
#1258=EDGE_CURVE('',#1044,#1043,#225,.T.);
#1259=EDGE_CURVE('',#1045,#1044,#226,.T.);
#1260=EDGE_CURVE('',#1042,#1045,#725,.F.);
#1261=EDGE_CURVE('',#1040,#1042,#227,.T.);
#1262=EDGE_CURVE('',#1045,#1046,#726,.F.);
#1263=EDGE_CURVE('',#1043,#1045,#228,.T.);
#1264=EDGE_CURVE('',#1047,#1043,#727,.T.);
#1265=EDGE_CURVE('',#1046,#1047,#229,.T.);
#1266=EDGE_CURVE('',#1048,#1049,#728,.T.);
#1267=EDGE_CURVE('',#1050,#1048,#230,.T.);
#1268=EDGE_CURVE('',#1051,#1050,#231,.T.);
#1269=EDGE_CURVE('',#1052,#1051,#729,.F.);
#1270=EDGE_CURVE('',#1053,#1052,#232,.T.);
#1271=EDGE_CURVE('',#1049,#1053,#233,.T.);
#1272=EDGE_CURVE('',#1054,#1048,#730,.T.);
#1273=EDGE_CURVE('',#1055,#1054,#234,.T.);
#1274=EDGE_CURVE('',#1056,#1055,#235,.T.);
#1275=EDGE_CURVE('',#1051,#1056,#731,.F.);
#1276=EDGE_CURVE('',#1048,#1051,#236,.T.);
#1277=EDGE_CURVE('',#1057,#1054,#732,.T.);
#1278=EDGE_CURVE('',#1058,#1057,#237,.T.);
#1279=EDGE_CURVE('',#1059,#1058,#238,.T.);
#1280=EDGE_CURVE('',#1056,#1059,#733,.F.);
#1281=EDGE_CURVE('',#1054,#1056,#239,.T.);
#1282=EDGE_CURVE('',#1059,#1060,#734,.F.);
#1283=EDGE_CURVE('',#1057,#1059,#240,.T.);
#1284=EDGE_CURVE('',#1061,#1057,#735,.T.);
#1285=EDGE_CURVE('',#1060,#1061,#241,.T.);
#1286=EDGE_CURVE('',#1062,#1063,#614,.T.);
#1287=EDGE_CURVE('',#1062,#1064,#736,.T.);
#1288=EDGE_CURVE('',#1064,#1065,#615,.T.);
#1289=EDGE_CURVE('',#1065,#1063,#737,.F.);
#1290=EDGE_CURVE('',#1066,#1067,#738,.T.);
#1291=EDGE_CURVE('',#1066,#1068,#616,.T.);
#1292=EDGE_CURVE('',#1069,#1068,#739,.F.);
#1293=EDGE_CURVE('',#1067,#1069,#617,.T.);
#1294=EDGE_CURVE('',#1070,#1070,#618,.T.);
#1295=EDGE_CURVE('',#1071,#1064,#740,.T.);
#1296=EDGE_CURVE('',#1072,#1071,#619,.F.);
#1297=EDGE_CURVE('',#1072,#1013,#741,.T.);
#1298=EDGE_CURVE('',#1073,#1012,#742,.T.);
#1299=EDGE_CURVE('',#1074,#1073,#620,.F.);
#1300=EDGE_CURVE('',#1074,#1031,#743,.T.);
#1301=EDGE_CURVE('',#1075,#1030,#744,.T.);
#1302=EDGE_CURVE('',#1076,#1075,#621,.F.);
#1303=EDGE_CURVE('',#1076,#1065,#745,.T.);
#1304=EDGE_CURVE('',#1077,#1077,#622,.T.);
#1305=EDGE_CURVE('',#1078,#1004,#746,.T.);
#1306=EDGE_CURVE('',#1079,#1078,#747,.T.);
#1307=EDGE_CURVE('',#1009,#1079,#748,.T.);
#1308=EDGE_CURVE('',#1080,#1011,#749,.T.);
#1309=EDGE_CURVE('',#1081,#1080,#750,.T.);
#1310=EDGE_CURVE('',#1067,#1081,#751,.T.);
#1311=EDGE_CURVE('',#1082,#1069,#752,.T.);
#1312=EDGE_CURVE('',#1083,#1082,#753,.T.);
#1313=EDGE_CURVE('',#1006,#1083,#754,.T.);
#1314=EDGE_CURVE('',#1077,#1070,#755,.T.);
#1315=EDGE_CURVE('',#1008,#1084,#756,.T.);
#1316=EDGE_CURVE('',#1084,#1085,#757,.T.);
#1317=EDGE_CURVE('',#1085,#1005,#758,.T.);
#1318=EDGE_CURVE('',#1007,#1086,#759,.T.);
#1319=EDGE_CURVE('',#1086,#1087,#760,.T.);
#1320=EDGE_CURVE('',#1087,#1068,#761,.T.);
#1321=EDGE_CURVE('',#1066,#1088,#762,.T.);
#1322=EDGE_CURVE('',#1088,#1089,#763,.T.);
#1323=EDGE_CURVE('',#1089,#1010,#764,.T.);
#1324=EDGE_CURVE('',#1090,#1090,#623,.T.);
#1325=EDGE_CURVE('',#1091,#1014,#765,.T.);
#1326=EDGE_CURVE('',#1092,#1091,#624,.F.);
#1327=EDGE_CURVE('',#1062,#1092,#766,.T.);
#1328=EDGE_CURVE('',#1093,#1063,#767,.T.);
#1329=EDGE_CURVE('',#1094,#1093,#625,.F.);
#1330=EDGE_CURVE('',#1033,#1094,#768,.T.);
#1331=EDGE_CURVE('',#1095,#1032,#769,.T.);
#1332=EDGE_CURVE('',#1096,#1095,#626,.F.);
#1333=EDGE_CURVE('',#1015,#1096,#770,.T.);
#1334=EDGE_CURVE('',#1097,#1097,#627,.T.);
#1335=EDGE_CURVE('',#1098,#1098,#628,.T.);
#1336=EDGE_CURVE('',#1097,#1053,#771,.T.);
#1337=EDGE_CURVE('',#1099,#1052,#772,.T.);
#1338=EDGE_CURVE('',#1099,#1100,#242,.T.);
#1339=EDGE_CURVE('',#1100,#1049,#773,.T.);
#1340=EDGE_CURVE('',#1101,#1101,#629,.T.);
#1341=EDGE_CURVE('',#1102,#1102,#630,.T.);
#1342=EDGE_CURVE('',#1101,#1050,#774,.T.);
#1343=EDGE_CURVE('',#1103,#1103,#631,.T.);
#1344=EDGE_CURVE('',#1104,#1104,#632,.T.);
#1345=EDGE_CURVE('',#1103,#1055,#775,.T.);
#1346=EDGE_CURVE('',#1105,#1105,#633,.T.);
#1347=EDGE_CURVE('',#1106,#1106,#634,.T.);
#1348=EDGE_CURVE('',#1105,#1058,#776,.T.);
#1349=EDGE_CURVE('',#1107,#1107,#635,.T.);
#1350=EDGE_CURVE('',#1108,#1108,#636,.T.);
#1351=EDGE_CURVE('',#1107,#1098,#777,.T.);
#1352=EDGE_CURVE('',#1109,#1109,#637,.T.);
#1353=EDGE_CURVE('',#1110,#1110,#638,.T.);
#1354=EDGE_CURVE('',#1109,#1102,#778,.T.);
#1355=EDGE_CURVE('',#1111,#1111,#639,.T.);
#1356=EDGE_CURVE('',#1112,#1112,#640,.T.);
#1357=EDGE_CURVE('',#1111,#1104,#779,.T.);
#1358=EDGE_CURVE('',#1113,#1113,#641,.F.);
#1359=EDGE_CURVE('',#1113,#1090,#780,.T.);
#1360=EDGE_CURVE('',#1114,#1115,#243,.T.);
#1361=EDGE_CURVE('',#1115,#1114,#244,.T.);
#1362=EDGE_CURVE('',#1116,#1117,#245,.T.);
#1363=EDGE_CURVE('',#1117,#1116,#246,.T.);
#1364=EDGE_CURVE('',#1118,#1119,#247,.T.);
#1365=EDGE_CURVE('',#1119,#1118,#248,.T.);
#1366=EDGE_CURVE('',#1120,#1121,#249,.T.);
#1367=EDGE_CURVE('',#1121,#1120,#250,.T.);
#1368=EDGE_CURVE('',#1122,#1123,#251,.T.);
#1369=EDGE_CURVE('',#1123,#1122,#252,.T.);
#1370=EDGE_CURVE('',#1124,#1125,#253,.T.);
#1371=EDGE_CURVE('',#1125,#1124,#254,.T.);
#1372=EDGE_CURVE('',#1126,#1127,#255,.T.);
#1373=EDGE_CURVE('',#1127,#1126,#256,.T.);
#1374=EDGE_CURVE('',#1128,#1129,#257,.T.);
#1375=EDGE_CURVE('',#1129,#1128,#258,.T.);
#1376=EDGE_CURVE('',#1130,#1131,#259,.T.);
#1377=EDGE_CURVE('',#1131,#1130,#260,.T.);
#1378=EDGE_CURVE('',#1132,#1133,#261,.T.);
#1379=EDGE_CURVE('',#1133,#1132,#262,.T.);
#1380=EDGE_CURVE('',#1134,#1135,#263,.T.);
#1381=EDGE_CURVE('',#1135,#1134,#264,.T.);
#1382=EDGE_CURVE('',#1136,#1137,#265,.T.);
#1383=EDGE_CURVE('',#1137,#1136,#266,.T.);
#1384=EDGE_CURVE('',#1138,#1138,#642,.T.);
#1385=EDGE_CURVE('',#1139,#1139,#643,.T.);
#1386=EDGE_CURVE('',#1138,#1106,#781,.T.);
#1387=EDGE_CURVE('',#1137,#1108,#782,.T.);
#1388=EDGE_CURVE('',#1135,#1110,#783,.T.);
#1389=EDGE_CURVE('',#1133,#1112,#784,.T.);
#1390=EDGE_CURVE('',#1131,#1139,#785,.T.);
#1391=EDGE_CURVE('',#1140,#1140,#644,.T.);
#1392=EDGE_CURVE('',#1141,#1141,#645,.T.);
#1393=EDGE_CURVE('',#1140,#1021,#786,.T.);
#1394=EDGE_CURVE('',#1142,#1020,#787,.T.);
#1395=EDGE_CURVE('',#1142,#1143,#267,.T.);
#1396=EDGE_CURVE('',#1143,#1017,#788,.T.);
#1397=EDGE_CURVE('',#1144,#1144,#646,.T.);
#1398=EDGE_CURVE('',#1145,#1145,#647,.T.);
#1399=EDGE_CURVE('',#1144,#1039,#789,.T.);
#1400=EDGE_CURVE('',#1146,#1038,#790,.T.);
#1401=EDGE_CURVE('',#1146,#1147,#268,.T.);
#1402=EDGE_CURVE('',#1147,#1035,#791,.T.);
#1403=EDGE_CURVE('',#1148,#1148,#648,.T.);
#1404=EDGE_CURVE('',#1149,#1149,#649,.T.);
#1405=EDGE_CURVE('',#1148,#1018,#792,.T.);
#1406=EDGE_CURVE('',#1150,#1150,#650,.T.);
#1407=EDGE_CURVE('',#1151,#1151,#651,.T.);
#1408=EDGE_CURVE('',#1150,#1036,#793,.T.);
#1409=EDGE_CURVE('',#1152,#1152,#652,.T.);
#1410=EDGE_CURVE('',#1153,#1153,#653,.T.);
#1411=EDGE_CURVE('',#1152,#1023,#794,.T.);
#1412=EDGE_CURVE('',#1154,#1154,#654,.T.);
#1413=EDGE_CURVE('',#1155,#1155,#655,.T.);
#1414=EDGE_CURVE('',#1154,#1041,#795,.T.);
#1415=EDGE_CURVE('',#1156,#1156,#656,.T.);
#1416=EDGE_CURVE('',#1157,#1157,#657,.T.);
#1417=EDGE_CURVE('',#1156,#1026,#796,.T.);
#1418=EDGE_CURVE('',#1158,#1158,#658,.T.);
#1419=EDGE_CURVE('',#1159,#1159,#659,.T.);
#1420=EDGE_CURVE('',#1158,#1044,#797,.T.);
#1421=EDGE_CURVE('',#1129,#1160,#798,.T.);
#1422=EDGE_CURVE('',#1160,#1160,#660,.F.);
#1423=EDGE_CURVE('',#1127,#1161,#799,.T.);
#1424=EDGE_CURVE('',#1161,#1161,#661,.F.);
#1425=EDGE_CURVE('',#1125,#1162,#800,.T.);
#1426=EDGE_CURVE('',#1162,#1162,#662,.F.);
#1427=EDGE_CURVE('',#1123,#1163,#801,.T.);
#1428=EDGE_CURVE('',#1163,#1163,#663,.F.);
#1429=EDGE_CURVE('',#1121,#1164,#802,.T.);
#1430=EDGE_CURVE('',#1164,#1164,#664,.F.);
#1431=EDGE_CURVE('',#1119,#1165,#803,.T.);
#1432=EDGE_CURVE('',#1165,#1165,#665,.F.);
#1433=EDGE_CURVE('',#1117,#1166,#804,.T.);
#1434=EDGE_CURVE('',#1166,#1166,#666,.F.);
#1435=EDGE_CURVE('',#1115,#1167,#805,.T.);
#1436=EDGE_CURVE('',#1167,#1167,#667,.F.);
#1437=EDGE_CURVE('',#1168,#1168,#668,.T.);
#1438=EDGE_CURVE('',#1168,#1141,#806,.T.);
#1439=EDGE_CURVE('',#1169,#1169,#669,.T.);
#1440=EDGE_CURVE('',#1169,#1145,#807,.T.);
#1441=EDGE_CURVE('',#1170,#1170,#670,.T.);
#1442=EDGE_CURVE('',#1170,#1149,#808,.T.);
#1443=EDGE_CURVE('',#1171,#1171,#671,.T.);
#1444=EDGE_CURVE('',#1171,#1151,#809,.T.);
#1445=EDGE_CURVE('',#1172,#1172,#672,.T.);
#1446=EDGE_CURVE('',#1172,#1153,#810,.T.);
#1447=EDGE_CURVE('',#1173,#1173,#673,.T.);
#1448=EDGE_CURVE('',#1173,#1155,#811,.T.);
#1449=EDGE_CURVE('',#1174,#1174,#674,.T.);
#1450=EDGE_CURVE('',#1174,#1157,#812,.T.);
#1451=EDGE_CURVE('',#1175,#1175,#675,.T.);
#1452=EDGE_CURVE('',#1175,#1159,#813,.T.);
#1453=EDGE_CURVE('',#1093,#1076,#814,.T.);
#1454=EDGE_CURVE('',#1075,#1094,#815,.F.);
#1455=EDGE_CURVE('',#1176,#1060,#816,.T.);
#1456=EDGE_CURVE('',#1176,#1099,#817,.T.);
#1457=EDGE_CURVE('',#1100,#1177,#818,.F.);
#1458=EDGE_CURVE('',#1177,#1061,#819,.T.);
#1459=EDGE_CURVE('',#1177,#1176,#269,.T.);
#1460=EDGE_CURVE('',#1095,#1074,#820,.T.);
#1461=EDGE_CURVE('',#1073,#1096,#821,.F.);
#1462=EDGE_CURVE('',#1178,#1046,#822,.T.);
#1463=EDGE_CURVE('',#1178,#1146,#823,.T.);
#1464=EDGE_CURVE('',#1147,#1179,#824,.F.);
#1465=EDGE_CURVE('',#1179,#1047,#825,.T.);
#1466=EDGE_CURVE('',#1179,#1178,#270,.T.);
#1467=EDGE_CURVE('',#1091,#1072,#826,.T.);
#1468=EDGE_CURVE('',#1071,#1092,#827,.F.);
#1469=EDGE_CURVE('',#1180,#1028,#828,.T.);
#1470=EDGE_CURVE('',#1180,#1142,#829,.T.);
#1471=EDGE_CURVE('',#1143,#1181,#830,.F.);
#1472=EDGE_CURVE('',#1181,#1029,#831,.T.);
#1473=EDGE_CURVE('',#1181,#1180,#271,.T.);
#1474=EDGE_CURVE('',#1087,#1082,#832,.T.);
#1475=EDGE_CURVE('',#1086,#1083,#833,.T.);
#1476=EDGE_CURVE('',#1089,#1080,#834,.T.);
#1477=EDGE_CURVE('',#1088,#1081,#835,.T.);
#1478=EDGE_CURVE('',#1085,#1078,#836,.T.);
#1479=EDGE_CURVE('',#1084,#1079,#837,.T.);
#1480=EDGE_CURVE('',#1182,#1182,#676,.T.);
#1481=EDGE_CURVE('',#1182,#1183,#838,.T.);
#1482=EDGE_CURVE('',#1183,#1183,#677,.T.);
#1483=EDGE_CURVE('',#1184,#1184,#678,.T.);
#1484=EDGE_CURVE('',#1185,#1185,#679,.T.);
#1485=EDGE_CURVE('',#1186,#1186,#680,.T.);
#1486=EDGE_CURVE('',#1186,#1187,#839,.T.);
#1487=EDGE_CURVE('',#1187,#1187,#681,.T.);
#1488=EDGE_CURVE('',#1187,#1185,#840,.T.);
#1489=EDGE_CURVE('',#1188,#1188,#682,.T.);
#1490=EDGE_CURVE('',#1184,#1188,#841,.T.);
#1491=EDGE_CURVE('',#1189,#1189,#683,.T.);
#1492=EDGE_CURVE('',#1189,#1190,#842,.T.);
#1493=EDGE_CURVE('',#1190,#1190,#684,.T.);
#1494=EDGE_CURVE('',#1191,#1191,#685,.T.);
#1495=EDGE_CURVE('',#1192,#1192,#686,.T.);
#1496=EDGE_CURVE('',#1193,#1193,#687,.T.);
#1497=EDGE_CURVE('',#1193,#1194,#843,.T.);
#1498=EDGE_CURVE('',#1194,#1194,#688,.T.);
#1499=EDGE_CURVE('',#1194,#1192,#844,.T.);
#1500=EDGE_CURVE('',#1195,#1195,#689,.T.);
#1501=EDGE_CURVE('',#1191,#1195,#845,.T.);
#1502=EDGE_CURVE('',#1196,#1196,#690,.T.);
#1503=EDGE_CURVE('',#1196,#1197,#846,.T.);
#1504=EDGE_CURVE('',#1197,#1197,#691,.T.);
#1505=EDGE_CURVE('',#1198,#1198,#692,.T.);
#1506=EDGE_CURVE('',#1199,#1199,#693,.T.);
#1507=EDGE_CURVE('',#1200,#1200,#694,.T.);
#1508=EDGE_CURVE('',#1200,#1201,#847,.T.);
#1509=EDGE_CURVE('',#1201,#1201,#695,.T.);
#1510=EDGE_CURVE('',#1201,#1199,#848,.T.);
#1511=EDGE_CURVE('',#1202,#1202,#696,.T.);
#1512=EDGE_CURVE('',#1198,#1202,#849,.T.);
#1513=EDGE_CURVE('',#1203,#1203,#697,.T.);
#1514=EDGE_CURVE('',#1203,#1204,#850,.T.);
#1515=EDGE_CURVE('',#1204,#1204,#698,.T.);
#1516=EDGE_CURVE('',#1205,#1205,#699,.T.);
#1517=EDGE_CURVE('',#1206,#1206,#700,.T.);
#1518=EDGE_CURVE('',#1207,#1207,#701,.T.);
#1519=EDGE_CURVE('',#1207,#1208,#851,.T.);
#1520=EDGE_CURVE('',#1208,#1208,#702,.T.);
#1521=EDGE_CURVE('',#1208,#1206,#852,.T.);
#1522=EDGE_CURVE('',#1209,#1209,#703,.T.);
#1523=EDGE_CURVE('',#1205,#1209,#853,.T.);
#1524=ORIENTED_EDGE('',*,*,#1210,.F.);
#1525=ORIENTED_EDGE('',*,*,#1211,.F.);
#1526=ORIENTED_EDGE('',*,*,#1212,.F.);
#1527=ORIENTED_EDGE('',*,*,#1213,.T.);
#1528=ORIENTED_EDGE('',*,*,#1214,.F.);
#1529=ORIENTED_EDGE('',*,*,#1215,.T.);
#1530=ORIENTED_EDGE('',*,*,#1216,.F.);
#1531=ORIENTED_EDGE('',*,*,#1217,.F.);
#1532=ORIENTED_EDGE('',*,*,#1218,.T.);
#1533=ORIENTED_EDGE('',*,*,#1219,.T.);
#1534=ORIENTED_EDGE('',*,*,#1220,.F.);
#1535=ORIENTED_EDGE('',*,*,#1221,.T.);
#1536=ORIENTED_EDGE('',*,*,#1222,.F.);
#1537=ORIENTED_EDGE('',*,*,#1223,.F.);
#1538=ORIENTED_EDGE('',*,*,#1224,.F.);
#1539=ORIENTED_EDGE('',*,*,#1225,.F.);
#1540=ORIENTED_EDGE('',*,*,#1226,.F.);
#1541=ORIENTED_EDGE('',*,*,#1227,.F.);
#1542=ORIENTED_EDGE('',*,*,#1228,.F.);
#1543=ORIENTED_EDGE('',*,*,#1229,.F.);
#1544=ORIENTED_EDGE('',*,*,#1230,.F.);
#1545=ORIENTED_EDGE('',*,*,#1231,.F.);
#1546=ORIENTED_EDGE('',*,*,#1232,.F.);
#1547=ORIENTED_EDGE('',*,*,#1233,.F.);
#1548=ORIENTED_EDGE('',*,*,#1234,.F.);
#1549=ORIENTED_EDGE('',*,*,#1235,.F.);
#1550=ORIENTED_EDGE('',*,*,#1236,.F.);
#1551=ORIENTED_EDGE('',*,*,#1237,.F.);
#1552=ORIENTED_EDGE('',*,*,#1238,.F.);
#1553=ORIENTED_EDGE('',*,*,#1239,.F.);
#1554=ORIENTED_EDGE('',*,*,#1240,.F.);
#1555=ORIENTED_EDGE('',*,*,#1241,.F.);
#1556=ORIENTED_EDGE('',*,*,#1242,.T.);
#1557=ORIENTED_EDGE('',*,*,#1243,.T.);
#1558=ORIENTED_EDGE('',*,*,#1244,.F.);
#1559=ORIENTED_EDGE('',*,*,#1245,.T.);
#1560=ORIENTED_EDGE('',*,*,#1246,.F.);
#1561=ORIENTED_EDGE('',*,*,#1247,.F.);
#1562=ORIENTED_EDGE('',*,*,#1248,.F.);
#1563=ORIENTED_EDGE('',*,*,#1249,.F.);
#1564=ORIENTED_EDGE('',*,*,#1250,.F.);
#1565=ORIENTED_EDGE('',*,*,#1251,.F.);
#1566=ORIENTED_EDGE('',*,*,#1252,.F.);
#1567=ORIENTED_EDGE('',*,*,#1253,.F.);
#1568=ORIENTED_EDGE('',*,*,#1254,.F.);
#1569=ORIENTED_EDGE('',*,*,#1255,.F.);
#1570=ORIENTED_EDGE('',*,*,#1256,.F.);
#1571=ORIENTED_EDGE('',*,*,#1257,.F.);
#1572=ORIENTED_EDGE('',*,*,#1258,.F.);
#1573=ORIENTED_EDGE('',*,*,#1259,.F.);
#1574=ORIENTED_EDGE('',*,*,#1260,.F.);
#1575=ORIENTED_EDGE('',*,*,#1261,.F.);
#1576=ORIENTED_EDGE('',*,*,#1262,.F.);
#1577=ORIENTED_EDGE('',*,*,#1263,.F.);
#1578=ORIENTED_EDGE('',*,*,#1264,.F.);
#1579=ORIENTED_EDGE('',*,*,#1265,.F.);
#1580=ORIENTED_EDGE('',*,*,#1266,.F.);
#1581=ORIENTED_EDGE('',*,*,#1267,.F.);
#1582=ORIENTED_EDGE('',*,*,#1268,.F.);
#1583=ORIENTED_EDGE('',*,*,#1269,.F.);
#1584=ORIENTED_EDGE('',*,*,#1270,.F.);
#1585=ORIENTED_EDGE('',*,*,#1271,.F.);
#1586=ORIENTED_EDGE('',*,*,#1272,.F.);
#1587=ORIENTED_EDGE('',*,*,#1273,.F.);
#1588=ORIENTED_EDGE('',*,*,#1274,.F.);
#1589=ORIENTED_EDGE('',*,*,#1275,.F.);
#1590=ORIENTED_EDGE('',*,*,#1276,.F.);
#1591=ORIENTED_EDGE('',*,*,#1277,.F.);
#1592=ORIENTED_EDGE('',*,*,#1278,.F.);
#1593=ORIENTED_EDGE('',*,*,#1279,.F.);
#1594=ORIENTED_EDGE('',*,*,#1280,.F.);
#1595=ORIENTED_EDGE('',*,*,#1281,.F.);
#1596=ORIENTED_EDGE('',*,*,#1282,.F.);
#1597=ORIENTED_EDGE('',*,*,#1283,.F.);
#1598=ORIENTED_EDGE('',*,*,#1284,.F.);
#1599=ORIENTED_EDGE('',*,*,#1285,.F.);
#1600=ORIENTED_EDGE('',*,*,#1286,.F.);
#1601=ORIENTED_EDGE('',*,*,#1287,.T.);
#1602=ORIENTED_EDGE('',*,*,#1288,.T.);
#1603=ORIENTED_EDGE('',*,*,#1289,.T.);
#1604=ORIENTED_EDGE('',*,*,#1290,.F.);
#1605=ORIENTED_EDGE('',*,*,#1291,.T.);
#1606=ORIENTED_EDGE('',*,*,#1292,.F.);
#1607=ORIENTED_EDGE('',*,*,#1293,.F.);
#1608=ORIENTED_EDGE('',*,*,#1294,.T.);
#1609=ORIENTED_EDGE('',*,*,#1288,.F.);
#1610=ORIENTED_EDGE('',*,*,#1295,.F.);
#1611=ORIENTED_EDGE('',*,*,#1296,.F.);
#1612=ORIENTED_EDGE('',*,*,#1297,.T.);
#1613=ORIENTED_EDGE('',*,*,#1218,.F.);
#1614=ORIENTED_EDGE('',*,*,#1298,.F.);
#1615=ORIENTED_EDGE('',*,*,#1299,.F.);
#1616=ORIENTED_EDGE('',*,*,#1300,.T.);
#1617=ORIENTED_EDGE('',*,*,#1242,.F.);
#1618=ORIENTED_EDGE('',*,*,#1301,.F.);
#1619=ORIENTED_EDGE('',*,*,#1302,.F.);
#1620=ORIENTED_EDGE('',*,*,#1303,.T.);
#1621=ORIENTED_EDGE('',*,*,#1304,.F.);
#1622=ORIENTED_EDGE('',*,*,#1211,.T.);
#1623=ORIENTED_EDGE('',*,*,#1305,.F.);
#1624=ORIENTED_EDGE('',*,*,#1306,.F.);
#1625=ORIENTED_EDGE('',*,*,#1307,.F.);
#1626=ORIENTED_EDGE('',*,*,#1217,.T.);
#1627=ORIENTED_EDGE('',*,*,#1308,.F.);
#1628=ORIENTED_EDGE('',*,*,#1309,.F.);
#1629=ORIENTED_EDGE('',*,*,#1310,.F.);
#1630=ORIENTED_EDGE('',*,*,#1293,.T.);
#1631=ORIENTED_EDGE('',*,*,#1311,.F.);
#1632=ORIENTED_EDGE('',*,*,#1312,.F.);
#1633=ORIENTED_EDGE('',*,*,#1313,.F.);
#1634=ORIENTED_EDGE('',*,*,#1304,.T.);
#1635=ORIENTED_EDGE('',*,*,#1314,.T.);
#1636=ORIENTED_EDGE('',*,*,#1294,.F.);
#1637=ORIENTED_EDGE('',*,*,#1314,.F.);
#1638=ORIENTED_EDGE('',*,*,#1215,.F.);
#1639=ORIENTED_EDGE('',*,*,#1315,.T.);
#1640=ORIENTED_EDGE('',*,*,#1316,.T.);
#1641=ORIENTED_EDGE('',*,*,#1317,.T.);
#1642=ORIENTED_EDGE('',*,*,#1213,.F.);
#1643=ORIENTED_EDGE('',*,*,#1318,.T.);
#1644=ORIENTED_EDGE('',*,*,#1319,.T.);
#1645=ORIENTED_EDGE('',*,*,#1320,.T.);
#1646=ORIENTED_EDGE('',*,*,#1291,.F.);
#1647=ORIENTED_EDGE('',*,*,#1321,.T.);
#1648=ORIENTED_EDGE('',*,*,#1322,.T.);
#1649=ORIENTED_EDGE('',*,*,#1323,.T.);
#1650=ORIENTED_EDGE('',*,*,#1324,.F.);
#1651=ORIENTED_EDGE('',*,*,#1325,.F.);
#1652=ORIENTED_EDGE('',*,*,#1326,.F.);
#1653=ORIENTED_EDGE('',*,*,#1327,.F.);
#1654=ORIENTED_EDGE('',*,*,#1286,.T.);
#1655=ORIENTED_EDGE('',*,*,#1328,.F.);
#1656=ORIENTED_EDGE('',*,*,#1329,.F.);
#1657=ORIENTED_EDGE('',*,*,#1330,.F.);
#1658=ORIENTED_EDGE('',*,*,#1244,.T.);
#1659=ORIENTED_EDGE('',*,*,#1331,.F.);
#1660=ORIENTED_EDGE('',*,*,#1332,.F.);
#1661=ORIENTED_EDGE('',*,*,#1333,.F.);
#1662=ORIENTED_EDGE('',*,*,#1220,.T.);
#1663=ORIENTED_EDGE('',*,*,#1334,.F.);
#1664=ORIENTED_EDGE('',*,*,#1335,.F.);
#1665=ORIENTED_EDGE('',*,*,#1334,.T.);
#1666=ORIENTED_EDGE('',*,*,#1336,.T.);
#1667=ORIENTED_EDGE('',*,*,#1270,.T.);
#1668=ORIENTED_EDGE('',*,*,#1337,.F.);
#1669=ORIENTED_EDGE('',*,*,#1338,.T.);
#1670=ORIENTED_EDGE('',*,*,#1339,.T.);
#1671=ORIENTED_EDGE('',*,*,#1271,.T.);
#1672=ORIENTED_EDGE('',*,*,#1336,.F.);
#1673=ORIENTED_EDGE('',*,*,#1340,.F.);
#1674=ORIENTED_EDGE('',*,*,#1341,.F.);
#1675=ORIENTED_EDGE('',*,*,#1340,.T.);
#1676=ORIENTED_EDGE('',*,*,#1342,.T.);
#1677=ORIENTED_EDGE('',*,*,#1267,.T.);
#1678=ORIENTED_EDGE('',*,*,#1276,.T.);
#1679=ORIENTED_EDGE('',*,*,#1268,.T.);
#1680=ORIENTED_EDGE('',*,*,#1342,.F.);
#1681=ORIENTED_EDGE('',*,*,#1343,.F.);
#1682=ORIENTED_EDGE('',*,*,#1344,.F.);
#1683=ORIENTED_EDGE('',*,*,#1343,.T.);
#1684=ORIENTED_EDGE('',*,*,#1345,.T.);
#1685=ORIENTED_EDGE('',*,*,#1273,.T.);
#1686=ORIENTED_EDGE('',*,*,#1281,.T.);
#1687=ORIENTED_EDGE('',*,*,#1274,.T.);
#1688=ORIENTED_EDGE('',*,*,#1345,.F.);
#1689=ORIENTED_EDGE('',*,*,#1346,.F.);
#1690=ORIENTED_EDGE('',*,*,#1347,.F.);
#1691=ORIENTED_EDGE('',*,*,#1346,.T.);
#1692=ORIENTED_EDGE('',*,*,#1348,.T.);
#1693=ORIENTED_EDGE('',*,*,#1278,.T.);
#1694=ORIENTED_EDGE('',*,*,#1283,.T.);
#1695=ORIENTED_EDGE('',*,*,#1279,.T.);
#1696=ORIENTED_EDGE('',*,*,#1348,.F.);
#1697=ORIENTED_EDGE('',*,*,#1349,.T.);
#1698=ORIENTED_EDGE('',*,*,#1350,.F.);
#1699=ORIENTED_EDGE('',*,*,#1349,.F.);
#1700=ORIENTED_EDGE('',*,*,#1351,.T.);
#1701=ORIENTED_EDGE('',*,*,#1335,.T.);
#1702=ORIENTED_EDGE('',*,*,#1351,.F.);
#1703=ORIENTED_EDGE('',*,*,#1352,.T.);
#1704=ORIENTED_EDGE('',*,*,#1353,.F.);
#1705=ORIENTED_EDGE('',*,*,#1352,.F.);
#1706=ORIENTED_EDGE('',*,*,#1354,.T.);
#1707=ORIENTED_EDGE('',*,*,#1341,.T.);
#1708=ORIENTED_EDGE('',*,*,#1354,.F.);
#1709=ORIENTED_EDGE('',*,*,#1355,.T.);
#1710=ORIENTED_EDGE('',*,*,#1356,.F.);
#1711=ORIENTED_EDGE('',*,*,#1355,.F.);
#1712=ORIENTED_EDGE('',*,*,#1357,.T.);
#1713=ORIENTED_EDGE('',*,*,#1344,.T.);
#1714=ORIENTED_EDGE('',*,*,#1357,.F.);
#1715=ORIENTED_EDGE('',*,*,#1358,.F.);
#1716=ORIENTED_EDGE('',*,*,#1359,.T.);
#1717=ORIENTED_EDGE('',*,*,#1324,.T.);
#1718=ORIENTED_EDGE('',*,*,#1359,.F.);
#1719=ORIENTED_EDGE('',*,*,#1360,.T.);
#1720=ORIENTED_EDGE('',*,*,#1361,.T.);
#1721=ORIENTED_EDGE('',*,*,#1362,.T.);
#1722=ORIENTED_EDGE('',*,*,#1363,.T.);
#1723=ORIENTED_EDGE('',*,*,#1364,.T.);
#1724=ORIENTED_EDGE('',*,*,#1365,.T.);
#1725=ORIENTED_EDGE('',*,*,#1366,.T.);
#1726=ORIENTED_EDGE('',*,*,#1367,.T.);
#1727=ORIENTED_EDGE('',*,*,#1368,.T.);
#1728=ORIENTED_EDGE('',*,*,#1369,.T.);
#1729=ORIENTED_EDGE('',*,*,#1370,.T.);
#1730=ORIENTED_EDGE('',*,*,#1371,.T.);
#1731=ORIENTED_EDGE('',*,*,#1372,.T.);
#1732=ORIENTED_EDGE('',*,*,#1373,.T.);
#1733=ORIENTED_EDGE('',*,*,#1374,.T.);
#1734=ORIENTED_EDGE('',*,*,#1375,.T.);
#1735=ORIENTED_EDGE('',*,*,#1376,.T.);
#1736=ORIENTED_EDGE('',*,*,#1377,.T.);
#1737=ORIENTED_EDGE('',*,*,#1378,.T.);
#1738=ORIENTED_EDGE('',*,*,#1379,.T.);
#1739=ORIENTED_EDGE('',*,*,#1380,.T.);
#1740=ORIENTED_EDGE('',*,*,#1381,.T.);
#1741=ORIENTED_EDGE('',*,*,#1382,.T.);
#1742=ORIENTED_EDGE('',*,*,#1383,.T.);
#1743=ORIENTED_EDGE('',*,*,#1358,.T.);
#1744=ORIENTED_EDGE('',*,*,#1384,.T.);
#1745=ORIENTED_EDGE('',*,*,#1385,.F.);
#1746=ORIENTED_EDGE('',*,*,#1384,.F.);
#1747=ORIENTED_EDGE('',*,*,#1386,.T.);
#1748=ORIENTED_EDGE('',*,*,#1347,.T.);
#1749=ORIENTED_EDGE('',*,*,#1386,.F.);
#1750=ORIENTED_EDGE('',*,*,#1382,.F.);
#1751=ORIENTED_EDGE('',*,*,#1383,.F.);
#1752=ORIENTED_EDGE('',*,*,#1387,.T.);
#1753=ORIENTED_EDGE('',*,*,#1350,.T.);
#1754=ORIENTED_EDGE('',*,*,#1387,.F.);
#1755=ORIENTED_EDGE('',*,*,#1380,.F.);
#1756=ORIENTED_EDGE('',*,*,#1381,.F.);
#1757=ORIENTED_EDGE('',*,*,#1388,.T.);
#1758=ORIENTED_EDGE('',*,*,#1353,.T.);
#1759=ORIENTED_EDGE('',*,*,#1388,.F.);
#1760=ORIENTED_EDGE('',*,*,#1378,.F.);
#1761=ORIENTED_EDGE('',*,*,#1379,.F.);
#1762=ORIENTED_EDGE('',*,*,#1389,.T.);
#1763=ORIENTED_EDGE('',*,*,#1356,.T.);
#1764=ORIENTED_EDGE('',*,*,#1389,.F.);
#1765=ORIENTED_EDGE('',*,*,#1376,.F.);
#1766=ORIENTED_EDGE('',*,*,#1377,.F.);
#1767=ORIENTED_EDGE('',*,*,#1390,.T.);
#1768=ORIENTED_EDGE('',*,*,#1385,.T.);
#1769=ORIENTED_EDGE('',*,*,#1390,.F.);
#1770=ORIENTED_EDGE('',*,*,#1391,.F.);
#1771=ORIENTED_EDGE('',*,*,#1392,.F.);
#1772=ORIENTED_EDGE('',*,*,#1391,.T.);
#1773=ORIENTED_EDGE('',*,*,#1393,.T.);
#1774=ORIENTED_EDGE('',*,*,#1226,.T.);
#1775=ORIENTED_EDGE('',*,*,#1394,.F.);
#1776=ORIENTED_EDGE('',*,*,#1395,.T.);
#1777=ORIENTED_EDGE('',*,*,#1396,.T.);
#1778=ORIENTED_EDGE('',*,*,#1227,.T.);
#1779=ORIENTED_EDGE('',*,*,#1393,.F.);
#1780=ORIENTED_EDGE('',*,*,#1397,.F.);
#1781=ORIENTED_EDGE('',*,*,#1398,.F.);
#1782=ORIENTED_EDGE('',*,*,#1397,.T.);
#1783=ORIENTED_EDGE('',*,*,#1399,.T.);
#1784=ORIENTED_EDGE('',*,*,#1250,.T.);
#1785=ORIENTED_EDGE('',*,*,#1400,.F.);
#1786=ORIENTED_EDGE('',*,*,#1401,.T.);
#1787=ORIENTED_EDGE('',*,*,#1402,.T.);
#1788=ORIENTED_EDGE('',*,*,#1251,.T.);
#1789=ORIENTED_EDGE('',*,*,#1399,.F.);
#1790=ORIENTED_EDGE('',*,*,#1403,.F.);
#1791=ORIENTED_EDGE('',*,*,#1404,.F.);
#1792=ORIENTED_EDGE('',*,*,#1403,.T.);
#1793=ORIENTED_EDGE('',*,*,#1405,.T.);
#1794=ORIENTED_EDGE('',*,*,#1223,.T.);
#1795=ORIENTED_EDGE('',*,*,#1232,.T.);
#1796=ORIENTED_EDGE('',*,*,#1224,.T.);
#1797=ORIENTED_EDGE('',*,*,#1405,.F.);
#1798=ORIENTED_EDGE('',*,*,#1406,.F.);
#1799=ORIENTED_EDGE('',*,*,#1407,.F.);
#1800=ORIENTED_EDGE('',*,*,#1406,.T.);
#1801=ORIENTED_EDGE('',*,*,#1408,.T.);
#1802=ORIENTED_EDGE('',*,*,#1247,.T.);
#1803=ORIENTED_EDGE('',*,*,#1256,.T.);
#1804=ORIENTED_EDGE('',*,*,#1248,.T.);
#1805=ORIENTED_EDGE('',*,*,#1408,.F.);
#1806=ORIENTED_EDGE('',*,*,#1409,.F.);
#1807=ORIENTED_EDGE('',*,*,#1410,.F.);
#1808=ORIENTED_EDGE('',*,*,#1409,.T.);
#1809=ORIENTED_EDGE('',*,*,#1411,.T.);
#1810=ORIENTED_EDGE('',*,*,#1229,.T.);
#1811=ORIENTED_EDGE('',*,*,#1237,.T.);
#1812=ORIENTED_EDGE('',*,*,#1230,.T.);
#1813=ORIENTED_EDGE('',*,*,#1411,.F.);
#1814=ORIENTED_EDGE('',*,*,#1412,.F.);
#1815=ORIENTED_EDGE('',*,*,#1413,.F.);
#1816=ORIENTED_EDGE('',*,*,#1412,.T.);
#1817=ORIENTED_EDGE('',*,*,#1414,.T.);
#1818=ORIENTED_EDGE('',*,*,#1253,.T.);
#1819=ORIENTED_EDGE('',*,*,#1261,.T.);
#1820=ORIENTED_EDGE('',*,*,#1254,.T.);
#1821=ORIENTED_EDGE('',*,*,#1414,.F.);
#1822=ORIENTED_EDGE('',*,*,#1415,.F.);
#1823=ORIENTED_EDGE('',*,*,#1416,.F.);
#1824=ORIENTED_EDGE('',*,*,#1415,.T.);
#1825=ORIENTED_EDGE('',*,*,#1417,.T.);
#1826=ORIENTED_EDGE('',*,*,#1234,.T.);
#1827=ORIENTED_EDGE('',*,*,#1239,.T.);
#1828=ORIENTED_EDGE('',*,*,#1235,.T.);
#1829=ORIENTED_EDGE('',*,*,#1417,.F.);
#1830=ORIENTED_EDGE('',*,*,#1418,.F.);
#1831=ORIENTED_EDGE('',*,*,#1419,.F.);
#1832=ORIENTED_EDGE('',*,*,#1418,.T.);
#1833=ORIENTED_EDGE('',*,*,#1420,.T.);
#1834=ORIENTED_EDGE('',*,*,#1258,.T.);
#1835=ORIENTED_EDGE('',*,*,#1263,.T.);
#1836=ORIENTED_EDGE('',*,*,#1259,.T.);
#1837=ORIENTED_EDGE('',*,*,#1420,.F.);
#1838=ORIENTED_EDGE('',*,*,#1374,.F.);
#1839=ORIENTED_EDGE('',*,*,#1375,.F.);
#1840=ORIENTED_EDGE('',*,*,#1421,.T.);
#1841=ORIENTED_EDGE('',*,*,#1422,.F.);
#1842=ORIENTED_EDGE('',*,*,#1421,.F.);
#1843=ORIENTED_EDGE('',*,*,#1372,.F.);
#1844=ORIENTED_EDGE('',*,*,#1373,.F.);
#1845=ORIENTED_EDGE('',*,*,#1423,.T.);
#1846=ORIENTED_EDGE('',*,*,#1424,.F.);
#1847=ORIENTED_EDGE('',*,*,#1423,.F.);
#1848=ORIENTED_EDGE('',*,*,#1370,.F.);
#1849=ORIENTED_EDGE('',*,*,#1371,.F.);
#1850=ORIENTED_EDGE('',*,*,#1425,.T.);
#1851=ORIENTED_EDGE('',*,*,#1426,.F.);
#1852=ORIENTED_EDGE('',*,*,#1425,.F.);
#1853=ORIENTED_EDGE('',*,*,#1368,.F.);
#1854=ORIENTED_EDGE('',*,*,#1369,.F.);
#1855=ORIENTED_EDGE('',*,*,#1427,.T.);
#1856=ORIENTED_EDGE('',*,*,#1428,.F.);
#1857=ORIENTED_EDGE('',*,*,#1427,.F.);
#1858=ORIENTED_EDGE('',*,*,#1366,.F.);
#1859=ORIENTED_EDGE('',*,*,#1367,.F.);
#1860=ORIENTED_EDGE('',*,*,#1429,.T.);
#1861=ORIENTED_EDGE('',*,*,#1430,.F.);
#1862=ORIENTED_EDGE('',*,*,#1429,.F.);
#1863=ORIENTED_EDGE('',*,*,#1364,.F.);
#1864=ORIENTED_EDGE('',*,*,#1365,.F.);
#1865=ORIENTED_EDGE('',*,*,#1431,.T.);
#1866=ORIENTED_EDGE('',*,*,#1432,.F.);
#1867=ORIENTED_EDGE('',*,*,#1431,.F.);
#1868=ORIENTED_EDGE('',*,*,#1362,.F.);
#1869=ORIENTED_EDGE('',*,*,#1363,.F.);
#1870=ORIENTED_EDGE('',*,*,#1433,.T.);
#1871=ORIENTED_EDGE('',*,*,#1434,.F.);
#1872=ORIENTED_EDGE('',*,*,#1433,.F.);
#1873=ORIENTED_EDGE('',*,*,#1360,.F.);
#1874=ORIENTED_EDGE('',*,*,#1361,.F.);
#1875=ORIENTED_EDGE('',*,*,#1435,.T.);
#1876=ORIENTED_EDGE('',*,*,#1436,.F.);
#1877=ORIENTED_EDGE('',*,*,#1435,.F.);
#1878=ORIENTED_EDGE('',*,*,#1437,.T.);
#1879=ORIENTED_EDGE('',*,*,#1424,.T.);
#1880=ORIENTED_EDGE('',*,*,#1437,.F.);
#1881=ORIENTED_EDGE('',*,*,#1438,.T.);
#1882=ORIENTED_EDGE('',*,*,#1392,.T.);
#1883=ORIENTED_EDGE('',*,*,#1438,.F.);
#1884=ORIENTED_EDGE('',*,*,#1439,.T.);
#1885=ORIENTED_EDGE('',*,*,#1422,.T.);
#1886=ORIENTED_EDGE('',*,*,#1439,.F.);
#1887=ORIENTED_EDGE('',*,*,#1440,.T.);
#1888=ORIENTED_EDGE('',*,*,#1398,.T.);
#1889=ORIENTED_EDGE('',*,*,#1440,.F.);
#1890=ORIENTED_EDGE('',*,*,#1441,.T.);
#1891=ORIENTED_EDGE('',*,*,#1428,.T.);
#1892=ORIENTED_EDGE('',*,*,#1441,.F.);
#1893=ORIENTED_EDGE('',*,*,#1442,.T.);
#1894=ORIENTED_EDGE('',*,*,#1404,.T.);
#1895=ORIENTED_EDGE('',*,*,#1442,.F.);
#1896=ORIENTED_EDGE('',*,*,#1443,.T.);
#1897=ORIENTED_EDGE('',*,*,#1426,.T.);
#1898=ORIENTED_EDGE('',*,*,#1443,.F.);
#1899=ORIENTED_EDGE('',*,*,#1444,.T.);
#1900=ORIENTED_EDGE('',*,*,#1407,.T.);
#1901=ORIENTED_EDGE('',*,*,#1444,.F.);
#1902=ORIENTED_EDGE('',*,*,#1445,.T.);
#1903=ORIENTED_EDGE('',*,*,#1432,.T.);
#1904=ORIENTED_EDGE('',*,*,#1445,.F.);
#1905=ORIENTED_EDGE('',*,*,#1446,.T.);
#1906=ORIENTED_EDGE('',*,*,#1410,.T.);
#1907=ORIENTED_EDGE('',*,*,#1446,.F.);
#1908=ORIENTED_EDGE('',*,*,#1447,.T.);
#1909=ORIENTED_EDGE('',*,*,#1430,.T.);
#1910=ORIENTED_EDGE('',*,*,#1447,.F.);
#1911=ORIENTED_EDGE('',*,*,#1448,.T.);
#1912=ORIENTED_EDGE('',*,*,#1413,.T.);
#1913=ORIENTED_EDGE('',*,*,#1448,.F.);
#1914=ORIENTED_EDGE('',*,*,#1449,.T.);
#1915=ORIENTED_EDGE('',*,*,#1436,.T.);
#1916=ORIENTED_EDGE('',*,*,#1449,.F.);
#1917=ORIENTED_EDGE('',*,*,#1450,.T.);
#1918=ORIENTED_EDGE('',*,*,#1416,.T.);
#1919=ORIENTED_EDGE('',*,*,#1450,.F.);
#1920=ORIENTED_EDGE('',*,*,#1451,.T.);
#1921=ORIENTED_EDGE('',*,*,#1434,.T.);
#1922=ORIENTED_EDGE('',*,*,#1451,.F.);
#1923=ORIENTED_EDGE('',*,*,#1452,.T.);
#1924=ORIENTED_EDGE('',*,*,#1419,.T.);
#1925=ORIENTED_EDGE('',*,*,#1452,.F.);
#1926=ORIENTED_EDGE('',*,*,#1303,.F.);
#1927=ORIENTED_EDGE('',*,*,#1453,.F.);
#1928=ORIENTED_EDGE('',*,*,#1328,.T.);
#1929=ORIENTED_EDGE('',*,*,#1289,.F.);
#1930=ORIENTED_EDGE('',*,*,#1330,.T.);
#1931=ORIENTED_EDGE('',*,*,#1454,.F.);
#1932=ORIENTED_EDGE('',*,*,#1301,.T.);
#1933=ORIENTED_EDGE('',*,*,#1245,.F.);
#1934=ORIENTED_EDGE('',*,*,#1269,.T.);
#1935=ORIENTED_EDGE('',*,*,#1275,.T.);
#1936=ORIENTED_EDGE('',*,*,#1280,.T.);
#1937=ORIENTED_EDGE('',*,*,#1282,.T.);
#1938=ORIENTED_EDGE('',*,*,#1455,.F.);
#1939=ORIENTED_EDGE('',*,*,#1456,.T.);
#1940=ORIENTED_EDGE('',*,*,#1337,.T.);
#1941=ORIENTED_EDGE('',*,*,#1284,.T.);
#1942=ORIENTED_EDGE('',*,*,#1277,.T.);
#1943=ORIENTED_EDGE('',*,*,#1272,.T.);
#1944=ORIENTED_EDGE('',*,*,#1266,.T.);
#1945=ORIENTED_EDGE('',*,*,#1339,.F.);
#1946=ORIENTED_EDGE('',*,*,#1457,.T.);
#1947=ORIENTED_EDGE('',*,*,#1458,.T.);
#1948=ORIENTED_EDGE('',*,*,#1285,.T.);
#1949=ORIENTED_EDGE('',*,*,#1458,.F.);
#1950=ORIENTED_EDGE('',*,*,#1459,.T.);
#1951=ORIENTED_EDGE('',*,*,#1455,.T.);
#1952=ORIENTED_EDGE('',*,*,#1329,.T.);
#1953=ORIENTED_EDGE('',*,*,#1453,.T.);
#1954=ORIENTED_EDGE('',*,*,#1302,.T.);
#1955=ORIENTED_EDGE('',*,*,#1454,.T.);
#1956=ORIENTED_EDGE('',*,*,#1457,.F.);
#1957=ORIENTED_EDGE('',*,*,#1338,.F.);
#1958=ORIENTED_EDGE('',*,*,#1456,.F.);
#1959=ORIENTED_EDGE('',*,*,#1459,.F.);
#1960=ORIENTED_EDGE('',*,*,#1300,.F.);
#1961=ORIENTED_EDGE('',*,*,#1460,.F.);
#1962=ORIENTED_EDGE('',*,*,#1331,.T.);
#1963=ORIENTED_EDGE('',*,*,#1243,.F.);
#1964=ORIENTED_EDGE('',*,*,#1333,.T.);
#1965=ORIENTED_EDGE('',*,*,#1461,.F.);
#1966=ORIENTED_EDGE('',*,*,#1298,.T.);
#1967=ORIENTED_EDGE('',*,*,#1221,.F.);
#1968=ORIENTED_EDGE('',*,*,#1249,.T.);
#1969=ORIENTED_EDGE('',*,*,#1255,.T.);
#1970=ORIENTED_EDGE('',*,*,#1260,.T.);
#1971=ORIENTED_EDGE('',*,*,#1262,.T.);
#1972=ORIENTED_EDGE('',*,*,#1462,.F.);
#1973=ORIENTED_EDGE('',*,*,#1463,.T.);
#1974=ORIENTED_EDGE('',*,*,#1400,.T.);
#1975=ORIENTED_EDGE('',*,*,#1264,.T.);
#1976=ORIENTED_EDGE('',*,*,#1257,.T.);
#1977=ORIENTED_EDGE('',*,*,#1252,.T.);
#1978=ORIENTED_EDGE('',*,*,#1246,.T.);
#1979=ORIENTED_EDGE('',*,*,#1402,.F.);
#1980=ORIENTED_EDGE('',*,*,#1464,.T.);
#1981=ORIENTED_EDGE('',*,*,#1465,.T.);
#1982=ORIENTED_EDGE('',*,*,#1265,.T.);
#1983=ORIENTED_EDGE('',*,*,#1465,.F.);
#1984=ORIENTED_EDGE('',*,*,#1466,.T.);
#1985=ORIENTED_EDGE('',*,*,#1462,.T.);
#1986=ORIENTED_EDGE('',*,*,#1332,.T.);
#1987=ORIENTED_EDGE('',*,*,#1460,.T.);
#1988=ORIENTED_EDGE('',*,*,#1299,.T.);
#1989=ORIENTED_EDGE('',*,*,#1461,.T.);
#1990=ORIENTED_EDGE('',*,*,#1464,.F.);
#1991=ORIENTED_EDGE('',*,*,#1401,.F.);
#1992=ORIENTED_EDGE('',*,*,#1463,.F.);
#1993=ORIENTED_EDGE('',*,*,#1466,.F.);
#1994=ORIENTED_EDGE('',*,*,#1297,.F.);
#1995=ORIENTED_EDGE('',*,*,#1467,.F.);
#1996=ORIENTED_EDGE('',*,*,#1325,.T.);
#1997=ORIENTED_EDGE('',*,*,#1219,.F.);
#1998=ORIENTED_EDGE('',*,*,#1327,.T.);
#1999=ORIENTED_EDGE('',*,*,#1468,.F.);
#2000=ORIENTED_EDGE('',*,*,#1295,.T.);
#2001=ORIENTED_EDGE('',*,*,#1287,.F.);
#2002=ORIENTED_EDGE('',*,*,#1225,.T.);
#2003=ORIENTED_EDGE('',*,*,#1231,.T.);
#2004=ORIENTED_EDGE('',*,*,#1236,.T.);
#2005=ORIENTED_EDGE('',*,*,#1238,.T.);
#2006=ORIENTED_EDGE('',*,*,#1469,.F.);
#2007=ORIENTED_EDGE('',*,*,#1470,.T.);
#2008=ORIENTED_EDGE('',*,*,#1394,.T.);
#2009=ORIENTED_EDGE('',*,*,#1240,.T.);
#2010=ORIENTED_EDGE('',*,*,#1233,.T.);
#2011=ORIENTED_EDGE('',*,*,#1228,.T.);
#2012=ORIENTED_EDGE('',*,*,#1222,.T.);
#2013=ORIENTED_EDGE('',*,*,#1396,.F.);
#2014=ORIENTED_EDGE('',*,*,#1471,.T.);
#2015=ORIENTED_EDGE('',*,*,#1472,.T.);
#2016=ORIENTED_EDGE('',*,*,#1241,.T.);
#2017=ORIENTED_EDGE('',*,*,#1472,.F.);
#2018=ORIENTED_EDGE('',*,*,#1473,.T.);
#2019=ORIENTED_EDGE('',*,*,#1469,.T.);
#2020=ORIENTED_EDGE('',*,*,#1326,.T.);
#2021=ORIENTED_EDGE('',*,*,#1467,.T.);
#2022=ORIENTED_EDGE('',*,*,#1296,.T.);
#2023=ORIENTED_EDGE('',*,*,#1468,.T.);
#2024=ORIENTED_EDGE('',*,*,#1471,.F.);
#2025=ORIENTED_EDGE('',*,*,#1395,.F.);
#2026=ORIENTED_EDGE('',*,*,#1470,.F.);
#2027=ORIENTED_EDGE('',*,*,#1473,.F.);
#2028=ORIENTED_EDGE('',*,*,#1292,.T.);
#2029=ORIENTED_EDGE('',*,*,#1320,.F.);
#2030=ORIENTED_EDGE('',*,*,#1474,.T.);
#2031=ORIENTED_EDGE('',*,*,#1311,.T.);
#2032=ORIENTED_EDGE('',*,*,#1212,.T.);
#2033=ORIENTED_EDGE('',*,*,#1313,.T.);
#2034=ORIENTED_EDGE('',*,*,#1475,.F.);
#2035=ORIENTED_EDGE('',*,*,#1318,.F.);
#2036=ORIENTED_EDGE('',*,*,#1475,.T.);
#2037=ORIENTED_EDGE('',*,*,#1312,.T.);
#2038=ORIENTED_EDGE('',*,*,#1474,.F.);
#2039=ORIENTED_EDGE('',*,*,#1319,.F.);
#2040=ORIENTED_EDGE('',*,*,#1216,.T.);
#2041=ORIENTED_EDGE('',*,*,#1323,.F.);
#2042=ORIENTED_EDGE('',*,*,#1476,.T.);
#2043=ORIENTED_EDGE('',*,*,#1308,.T.);
#2044=ORIENTED_EDGE('',*,*,#1290,.T.);
#2045=ORIENTED_EDGE('',*,*,#1310,.T.);
#2046=ORIENTED_EDGE('',*,*,#1477,.F.);
#2047=ORIENTED_EDGE('',*,*,#1321,.F.);
#2048=ORIENTED_EDGE('',*,*,#1477,.T.);
#2049=ORIENTED_EDGE('',*,*,#1309,.T.);
#2050=ORIENTED_EDGE('',*,*,#1476,.F.);
#2051=ORIENTED_EDGE('',*,*,#1322,.F.);
#2052=ORIENTED_EDGE('',*,*,#1210,.T.);
#2053=ORIENTED_EDGE('',*,*,#1317,.F.);
#2054=ORIENTED_EDGE('',*,*,#1478,.T.);
#2055=ORIENTED_EDGE('',*,*,#1305,.T.);
#2056=ORIENTED_EDGE('',*,*,#1214,.T.);
#2057=ORIENTED_EDGE('',*,*,#1307,.T.);
#2058=ORIENTED_EDGE('',*,*,#1479,.F.);
#2059=ORIENTED_EDGE('',*,*,#1315,.F.);
#2060=ORIENTED_EDGE('',*,*,#1479,.T.);
#2061=ORIENTED_EDGE('',*,*,#1306,.T.);
#2062=ORIENTED_EDGE('',*,*,#1478,.F.);
#2063=ORIENTED_EDGE('',*,*,#1316,.F.);
#2064=ORIENTED_EDGE('',*,*,#1480,.T.);
#2065=ORIENTED_EDGE('',*,*,#1481,.T.);
#2066=ORIENTED_EDGE('',*,*,#1482,.F.);
#2067=ORIENTED_EDGE('',*,*,#1481,.F.);
#2068=ORIENTED_EDGE('',*,*,#1482,.T.);
#2069=ORIENTED_EDGE('',*,*,#1483,.F.);
#2070=ORIENTED_EDGE('',*,*,#1480,.F.);
#2071=ORIENTED_EDGE('',*,*,#1484,.F.);
#2072=ORIENTED_EDGE('',*,*,#1485,.T.);
#2073=ORIENTED_EDGE('',*,*,#1486,.T.);
#2074=ORIENTED_EDGE('',*,*,#1487,.T.);
#2075=ORIENTED_EDGE('',*,*,#1486,.F.);
#2076=ORIENTED_EDGE('',*,*,#1487,.F.);
#2077=ORIENTED_EDGE('',*,*,#1488,.T.);
#2078=ORIENTED_EDGE('',*,*,#1484,.T.);
#2079=ORIENTED_EDGE('',*,*,#1488,.F.);
#2080=ORIENTED_EDGE('',*,*,#1489,.T.);
#2081=ORIENTED_EDGE('',*,*,#1485,.F.);
#2082=ORIENTED_EDGE('',*,*,#1483,.T.);
#2083=ORIENTED_EDGE('',*,*,#1490,.T.);
#2084=ORIENTED_EDGE('',*,*,#1489,.F.);
#2085=ORIENTED_EDGE('',*,*,#1490,.F.);
#2086=ORIENTED_EDGE('',*,*,#1491,.T.);
#2087=ORIENTED_EDGE('',*,*,#1492,.T.);
#2088=ORIENTED_EDGE('',*,*,#1493,.F.);
#2089=ORIENTED_EDGE('',*,*,#1492,.F.);
#2090=ORIENTED_EDGE('',*,*,#1493,.T.);
#2091=ORIENTED_EDGE('',*,*,#1494,.F.);
#2092=ORIENTED_EDGE('',*,*,#1491,.F.);
#2093=ORIENTED_EDGE('',*,*,#1495,.F.);
#2094=ORIENTED_EDGE('',*,*,#1496,.T.);
#2095=ORIENTED_EDGE('',*,*,#1497,.T.);
#2096=ORIENTED_EDGE('',*,*,#1498,.T.);
#2097=ORIENTED_EDGE('',*,*,#1497,.F.);
#2098=ORIENTED_EDGE('',*,*,#1498,.F.);
#2099=ORIENTED_EDGE('',*,*,#1499,.T.);
#2100=ORIENTED_EDGE('',*,*,#1495,.T.);
#2101=ORIENTED_EDGE('',*,*,#1499,.F.);
#2102=ORIENTED_EDGE('',*,*,#1500,.T.);
#2103=ORIENTED_EDGE('',*,*,#1496,.F.);
#2104=ORIENTED_EDGE('',*,*,#1494,.T.);
#2105=ORIENTED_EDGE('',*,*,#1501,.T.);
#2106=ORIENTED_EDGE('',*,*,#1500,.F.);
#2107=ORIENTED_EDGE('',*,*,#1501,.F.);
#2108=ORIENTED_EDGE('',*,*,#1502,.T.);
#2109=ORIENTED_EDGE('',*,*,#1503,.T.);
#2110=ORIENTED_EDGE('',*,*,#1504,.F.);
#2111=ORIENTED_EDGE('',*,*,#1503,.F.);
#2112=ORIENTED_EDGE('',*,*,#1504,.T.);
#2113=ORIENTED_EDGE('',*,*,#1505,.F.);
#2114=ORIENTED_EDGE('',*,*,#1502,.F.);
#2115=ORIENTED_EDGE('',*,*,#1506,.F.);
#2116=ORIENTED_EDGE('',*,*,#1507,.T.);
#2117=ORIENTED_EDGE('',*,*,#1508,.T.);
#2118=ORIENTED_EDGE('',*,*,#1509,.T.);
#2119=ORIENTED_EDGE('',*,*,#1508,.F.);
#2120=ORIENTED_EDGE('',*,*,#1509,.F.);
#2121=ORIENTED_EDGE('',*,*,#1510,.T.);
#2122=ORIENTED_EDGE('',*,*,#1506,.T.);
#2123=ORIENTED_EDGE('',*,*,#1510,.F.);
#2124=ORIENTED_EDGE('',*,*,#1511,.T.);
#2125=ORIENTED_EDGE('',*,*,#1507,.F.);
#2126=ORIENTED_EDGE('',*,*,#1505,.T.);
#2127=ORIENTED_EDGE('',*,*,#1512,.T.);
#2128=ORIENTED_EDGE('',*,*,#1511,.F.);
#2129=ORIENTED_EDGE('',*,*,#1512,.F.);
#2130=ORIENTED_EDGE('',*,*,#1513,.F.);
#2131=ORIENTED_EDGE('',*,*,#1514,.T.);
#2132=ORIENTED_EDGE('',*,*,#1515,.T.);
#2133=ORIENTED_EDGE('',*,*,#1514,.F.);
#2134=ORIENTED_EDGE('',*,*,#1515,.F.);
#2135=ORIENTED_EDGE('',*,*,#1516,.F.);
#2136=ORIENTED_EDGE('',*,*,#1513,.T.);
#2137=ORIENTED_EDGE('',*,*,#1517,.F.);
#2138=ORIENTED_EDGE('',*,*,#1518,.F.);
#2139=ORIENTED_EDGE('',*,*,#1519,.T.);
#2140=ORIENTED_EDGE('',*,*,#1520,.T.);
#2141=ORIENTED_EDGE('',*,*,#1519,.F.);
#2142=ORIENTED_EDGE('',*,*,#1520,.F.);
#2143=ORIENTED_EDGE('',*,*,#1521,.T.);
#2144=ORIENTED_EDGE('',*,*,#1517,.T.);
#2145=ORIENTED_EDGE('',*,*,#1521,.F.);
#2146=ORIENTED_EDGE('',*,*,#1522,.T.);
#2147=ORIENTED_EDGE('',*,*,#1518,.T.);
#2148=ORIENTED_EDGE('',*,*,#1516,.T.);
#2149=ORIENTED_EDGE('',*,*,#1523,.T.);
#2150=ORIENTED_EDGE('',*,*,#1522,.F.);
#2151=ORIENTED_EDGE('',*,*,#1523,.F.);
#2152=CYLINDRICAL_SURFACE('',#2426,15.);
#2153=CYLINDRICAL_SURFACE('',#2429,15.);
#2154=CYLINDRICAL_SURFACE('',#2432,15.);
#2155=CYLINDRICAL_SURFACE('',#2435,15.);
#2156=CYLINDRICAL_SURFACE('',#2436,15.);
#2157=CYLINDRICAL_SURFACE('',#2437,15.);
#2158=CYLINDRICAL_SURFACE('',#2438,15.);
#2159=CYLINDRICAL_SURFACE('',#2439,15.);
#2160=CYLINDRICAL_SURFACE('',#2442,15.);
#2161=CYLINDRICAL_SURFACE('',#2443,15.);
#2162=CYLINDRICAL_SURFACE('',#2444,15.);
#2163=CYLINDRICAL_SURFACE('',#2445,15.);
#2164=CYLINDRICAL_SURFACE('',#2446,15.);
#2165=CYLINDRICAL_SURFACE('',#2447,15.);
#2166=CYLINDRICAL_SURFACE('',#2448,15.);
#2167=CYLINDRICAL_SURFACE('',#2449,15.);
#2168=CYLINDRICAL_SURFACE('',#2450,15.);
#2169=CYLINDRICAL_SURFACE('',#2453,15.);
#2170=CYLINDRICAL_SURFACE('',#2463,17.);
#2171=CYLINDRICAL_SURFACE('',#2473,4.00000000000012);
#2172=CYLINDRICAL_SURFACE('',#2477,4.00000000000001);
#2173=CYLINDRICAL_SURFACE('',#2481,4.00000000000001);
#2174=CYLINDRICAL_SURFACE('',#2485,4.);
#2175=CYLINDRICAL_SURFACE('',#2489,3.50000000000012);
#2176=CYLINDRICAL_SURFACE('',#2493,3.5);
#2177=CYLINDRICAL_SURFACE('',#2497,3.49999999999992);
#2178=CYLINDRICAL_SURFACE('',#2498,12.9999999999984);
#2179=CYLINDRICAL_SURFACE('',#2504,3.49999999999998);
#2180=CYLINDRICAL_SURFACE('',#2505,2.80000000000012);
#2181=CYLINDRICAL_SURFACE('',#2506,2.79999999999998);
#2182=CYLINDRICAL_SURFACE('',#2507,2.79999999999991);
#2183=CYLINDRICAL_SURFACE('',#2508,2.79999999999999);
#2184=CYLINDRICAL_SURFACE('',#2512,4.00000000000012);
#2185=CYLINDRICAL_SURFACE('',#2516,4.00000000000012);
#2186=CYLINDRICAL_SURFACE('',#2520,4.00000000000001);
#2187=CYLINDRICAL_SURFACE('',#2524,4.00000000000001);
#2188=CYLINDRICAL_SURFACE('',#2528,4.00000000000001);
#2189=CYLINDRICAL_SURFACE('',#2532,4.00000000000001);
#2190=CYLINDRICAL_SURFACE('',#2536,4.);
#2191=CYLINDRICAL_SURFACE('',#2540,4.);
#2192=CYLINDRICAL_SURFACE('',#2541,2.80000000000012);
#2193=CYLINDRICAL_SURFACE('',#2543,2.80000000000012);
#2194=CYLINDRICAL_SURFACE('',#2545,2.79999999999998);
#2195=CYLINDRICAL_SURFACE('',#2547,2.79999999999998);
#2196=CYLINDRICAL_SURFACE('',#2549,2.79999999999991);
#2197=CYLINDRICAL_SURFACE('',#2551,2.79999999999991);
#2198=CYLINDRICAL_SURFACE('',#2553,2.79999999999999);
#2199=CYLINDRICAL_SURFACE('',#2555,2.79999999999999);
#2200=CYLINDRICAL_SURFACE('',#2559,3.50000000000012);
#2201=CYLINDRICAL_SURFACE('',#2562,3.50000000000012);
#2202=CYLINDRICAL_SURFACE('',#2565,3.5);
#2203=CYLINDRICAL_SURFACE('',#2568,3.5);
#2204=CYLINDRICAL_SURFACE('',#2571,3.49999999999992);
#2205=CYLINDRICAL_SURFACE('',#2574,3.49999999999992);
#2206=CYLINDRICAL_SURFACE('',#2577,3.49999999999998);
#2207=CYLINDRICAL_SURFACE('',#2580,3.49999999999998);
#2208=CYLINDRICAL_SURFACE('',#2585,14.5);
#2209=CYLINDRICAL_SURFACE('',#2590,14.5);
#2210=CYLINDRICAL_SURFACE('',#2595,14.5);
#2211=CYLINDRICAL_SURFACE('',#2606,4.00000000000001);
#2212=CYLINDRICAL_SURFACE('',#2613,0.899999999999993);
#2213=CYLINDRICAL_SURFACE('',#2619,3.50000000000001);
#2214=CYLINDRICAL_SURFACE('',#2621,3.99999999999999);
#2215=CYLINDRICAL_SURFACE('',#2628,0.899999999999993);
#2216=CYLINDRICAL_SURFACE('',#2634,3.49999999999999);
#2217=CYLINDRICAL_SURFACE('',#2636,4.);
#2218=CYLINDRICAL_SURFACE('',#2643,0.899999999999989);
#2219=CYLINDRICAL_SURFACE('',#2649,3.49999999999993);
#2220=CYLINDRICAL_SURFACE('',#2651,4.00000000000013);
#2221=CYLINDRICAL_SURFACE('',#2658,0.899999999999984);
#2222=CYLINDRICAL_SURFACE('',#2664,3.50000000000012);
#2223=ADVANCED_FACE('',(#272),#2152,.F.);
#2224=ADVANCED_FACE('',(#273),#2153,.F.);
#2225=ADVANCED_FACE('',(#274),#2154,.T.);
#2226=ADVANCED_FACE('',(#275),#2155,.T.);
#2227=ADVANCED_FACE('',(#276),#2156,.T.);
#2228=ADVANCED_FACE('',(#277),#2157,.T.);
#2229=ADVANCED_FACE('',(#278),#2158,.T.);
#2230=ADVANCED_FACE('',(#279),#2159,.T.);
#2231=ADVANCED_FACE('',(#280),#2160,.T.);
#2232=ADVANCED_FACE('',(#281),#2161,.T.);
#2233=ADVANCED_FACE('',(#282),#2162,.T.);
#2234=ADVANCED_FACE('',(#283),#2163,.T.);
#2235=ADVANCED_FACE('',(#284),#2164,.T.);
#2236=ADVANCED_FACE('',(#285),#2165,.T.);
#2237=ADVANCED_FACE('',(#286),#2166,.T.);
#2238=ADVANCED_FACE('',(#287),#2167,.T.);
#2239=ADVANCED_FACE('',(#288),#2168,.T.);
#2240=ADVANCED_FACE('',(#289),#2169,.F.);
#2241=ADVANCED_FACE('',(#290,#90),#144,.T.);
#2242=ADVANCED_FACE('',(#291,#91),#145,.F.);
#2243=ADVANCED_FACE('',(#292),#2170,.T.);
#2244=ADVANCED_FACE('',(#293,#92),#146,.F.);
#2245=ADVANCED_FACE('',(#294),#147,.T.);
#2246=ADVANCED_FACE('',(#295,#93),#148,.F.);
#2247=ADVANCED_FACE('',(#296),#2171,.T.);
#2248=ADVANCED_FACE('',(#297,#94),#149,.F.);
#2249=ADVANCED_FACE('',(#298),#2172,.T.);
#2250=ADVANCED_FACE('',(#299,#95),#150,.F.);
#2251=ADVANCED_FACE('',(#300),#2173,.T.);
#2252=ADVANCED_FACE('',(#301,#96),#151,.F.);
#2253=ADVANCED_FACE('',(#302),#2174,.T.);
#2254=ADVANCED_FACE('',(#303,#97),#152,.T.);
#2255=ADVANCED_FACE('',(#304),#2175,.F.);
#2256=ADVANCED_FACE('',(#305,#98),#153,.T.);
#2257=ADVANCED_FACE('',(#306),#2176,.F.);
#2258=ADVANCED_FACE('',(#307,#99),#154,.T.);
#2259=ADVANCED_FACE('',(#308),#2177,.F.);
#2260=ADVANCED_FACE('',(#309,#100,#101,#102,#103,#104,#105,#106,#107,#108,
#109,#110,#111),#2178,.F.);
#2261=ADVANCED_FACE('',(#310),#155,.F.);
#2262=ADVANCED_FACE('',(#311,#112),#156,.T.);
#2263=ADVANCED_FACE('',(#312),#2179,.F.);
#2264=ADVANCED_FACE('',(#313),#2180,.F.);
#2265=ADVANCED_FACE('',(#314),#2181,.F.);
#2266=ADVANCED_FACE('',(#315),#2182,.F.);
#2267=ADVANCED_FACE('',(#316),#2183,.F.);
#2268=ADVANCED_FACE('',(#317,#113),#157,.F.);
#2269=ADVANCED_FACE('',(#318),#2184,.T.);
#2270=ADVANCED_FACE('',(#319,#114),#158,.F.);
#2271=ADVANCED_FACE('',(#320),#2185,.T.);
#2272=ADVANCED_FACE('',(#321,#115),#159,.F.);
#2273=ADVANCED_FACE('',(#322),#2186,.T.);
#2274=ADVANCED_FACE('',(#323,#116),#160,.F.);
#2275=ADVANCED_FACE('',(#324),#2187,.T.);
#2276=ADVANCED_FACE('',(#325,#117),#161,.F.);
#2277=ADVANCED_FACE('',(#326),#2188,.T.);
#2278=ADVANCED_FACE('',(#327,#118),#162,.F.);
#2279=ADVANCED_FACE('',(#328),#2189,.T.);
#2280=ADVANCED_FACE('',(#329,#119),#163,.F.);
#2281=ADVANCED_FACE('',(#330),#2190,.T.);
#2282=ADVANCED_FACE('',(#331,#120),#164,.F.);
#2283=ADVANCED_FACE('',(#332),#2191,.T.);
#2284=ADVANCED_FACE('',(#333),#2192,.F.);
#2285=ADVANCED_FACE('',(#334),#2193,.F.);
#2286=ADVANCED_FACE('',(#335),#2194,.F.);
#2287=ADVANCED_FACE('',(#336),#2195,.F.);
#2288=ADVANCED_FACE('',(#337),#2196,.F.);
#2289=ADVANCED_FACE('',(#338),#2197,.F.);
#2290=ADVANCED_FACE('',(#339),#2198,.F.);
#2291=ADVANCED_FACE('',(#340),#2199,.F.);
#2292=ADVANCED_FACE('',(#341,#121),#165,.T.);
#2293=ADVANCED_FACE('',(#342),#2200,.F.);
#2294=ADVANCED_FACE('',(#343,#122),#166,.T.);
#2295=ADVANCED_FACE('',(#344),#2201,.F.);
#2296=ADVANCED_FACE('',(#345,#123),#167,.T.);
#2297=ADVANCED_FACE('',(#346),#2202,.F.);
#2298=ADVANCED_FACE('',(#347,#124),#168,.T.);
#2299=ADVANCED_FACE('',(#348),#2203,.F.);
#2300=ADVANCED_FACE('',(#349,#125),#169,.T.);
#2301=ADVANCED_FACE('',(#350),#2204,.F.);
#2302=ADVANCED_FACE('',(#351,#126),#170,.T.);
#2303=ADVANCED_FACE('',(#352),#2205,.F.);
#2304=ADVANCED_FACE('',(#353,#127),#171,.T.);
#2305=ADVANCED_FACE('',(#354),#2206,.F.);
#2306=ADVANCED_FACE('',(#355,#128),#172,.T.);
#2307=ADVANCED_FACE('',(#356),#2207,.F.);
#2308=ADVANCED_FACE('',(#357),#173,.F.);
#2309=ADVANCED_FACE('',(#358),#174,.F.);
#2310=ADVANCED_FACE('',(#359),#175,.T.);
#2311=ADVANCED_FACE('',(#360),#176,.T.);
#2312=ADVANCED_FACE('',(#361),#87,.T.);
#2313=ADVANCED_FACE('',(#362,#129),#2208,.T.);
#2314=ADVANCED_FACE('',(#363),#177,.F.);
#2315=ADVANCED_FACE('',(#364),#178,.F.);
#2316=ADVANCED_FACE('',(#365),#179,.T.);
#2317=ADVANCED_FACE('',(#366),#180,.T.);
#2318=ADVANCED_FACE('',(#367),#88,.T.);
#2319=ADVANCED_FACE('',(#368,#130),#2209,.T.);
#2320=ADVANCED_FACE('',(#369),#181,.F.);
#2321=ADVANCED_FACE('',(#370),#182,.F.);
#2322=ADVANCED_FACE('',(#371),#183,.T.);
#2323=ADVANCED_FACE('',(#372),#184,.T.);
#2324=ADVANCED_FACE('',(#373),#89,.T.);
#2325=ADVANCED_FACE('',(#374,#131),#2210,.T.);
#2326=ADVANCED_FACE('',(#375),#185,.F.);
#2327=ADVANCED_FACE('',(#376),#186,.F.);
#2328=ADVANCED_FACE('',(#377),#187,.F.);
#2329=ADVANCED_FACE('',(#378),#188,.F.);
#2330=ADVANCED_FACE('',(#379),#189,.F.);
#2331=ADVANCED_FACE('',(#380),#190,.F.);
#2332=ADVANCED_FACE('',(#381),#191,.F.);
#2333=ADVANCED_FACE('',(#382),#192,.F.);
#2334=ADVANCED_FACE('',(#383),#193,.F.);
#2335=ADVANCED_FACE('',(#384),#2211,.T.);
#2336=ADVANCED_FACE('',(#385,#132),#194,.T.);
#2337=ADVANCED_FACE('',(#386,#133),#195,.F.);
#2338=ADVANCED_FACE('',(#387),#2212,.F.);
#2339=ADVANCED_FACE('',(#388),#63,.F.);
#2340=ADVANCED_FACE('',(#389,#134),#196,.T.);
#2341=ADVANCED_FACE('',(#390),#2213,.T.);
#2342=ADVANCED_FACE('',(#391),#2214,.T.);
#2343=ADVANCED_FACE('',(#392,#135),#197,.T.);
#2344=ADVANCED_FACE('',(#393,#136),#198,.F.);
#2345=ADVANCED_FACE('',(#394),#2215,.F.);
#2346=ADVANCED_FACE('',(#395),#64,.F.);
#2347=ADVANCED_FACE('',(#396,#137),#199,.T.);
#2348=ADVANCED_FACE('',(#397),#2216,.T.);
#2349=ADVANCED_FACE('',(#398),#2217,.T.);
#2350=ADVANCED_FACE('',(#399,#138),#200,.T.);
#2351=ADVANCED_FACE('',(#400,#139),#201,.F.);
#2352=ADVANCED_FACE('',(#401),#2218,.F.);
#2353=ADVANCED_FACE('',(#402),#65,.F.);
#2354=ADVANCED_FACE('',(#403,#140),#202,.T.);
#2355=ADVANCED_FACE('',(#404),#2219,.T.);
#2356=ADVANCED_FACE('',(#405),#2220,.T.);
#2357=ADVANCED_FACE('',(#406,#141),#203,.F.);
#2358=ADVANCED_FACE('',(#407,#142),#204,.T.);
#2359=ADVANCED_FACE('',(#408),#2221,.F.);
#2360=ADVANCED_FACE('',(#409),#66,.F.);
#2361=ADVANCED_FACE('',(#410,#143),#205,.T.);
#2362=ADVANCED_FACE('',(#411),#2222,.T.);
#2363=CLOSED_SHELL('',(#2223,#2224,#2225,#2226,#2227,#2228,#2229,#2230,
#2231,#2232,#2233,#2234,#2235,#2236,#2237,#2238,#2239,#2240,#2241,#2242,
#2243,#2244,#2245,#2246,#2247,#2248,#2249,#2250,#2251,#2252,#2253,#2254,
#2255,#2256,#2257,#2258,#2259,#2260,#2261,#2262,#2263,#2264,#2265,#2266,
#2267,#2268,#2269,#2270,#2271,#2272,#2273,#2274,#2275,#2276,#2277,#2278,
#2279,#2280,#2281,#2282,#2283,#2284,#2285,#2286,#2287,#2288,#2289,#2290,
#2291,#2292,#2293,#2294,#2295,#2296,#2297,#2298,#2299,#2300,#2301,#2302,
#2303,#2304,#2305,#2306,#2307,#2308,#2309,#2310,#2311,#2312,#2313,#2314,
#2315,#2316,#2317,#2318,#2319,#2320,#2321,#2322,#2323,#2324,#2325,#2326,
#2327,#2328,#2329,#2330,#2331,#2332,#2333,#2334));
#2364=CLOSED_SHELL('',(#2335,#2336,#2337,#2338,#2339,#2340,#2341));
#2365=CLOSED_SHELL('',(#2342,#2343,#2344,#2345,#2346,#2347,#2348));
#2366=CLOSED_SHELL('',(#2349,#2350,#2351,#2352,#2353,#2354,#2355));
#2367=CLOSED_SHELL('',(#2356,#2357,#2358,#2359,#2360,#2361,#2362));
#2368=DERIVED_UNIT_ELEMENT(#2378,1.);
#2369=DERIVED_UNIT_ELEMENT(#5185,-3.);
#2370=DERIVED_UNIT_ELEMENT(#2378,1.);
#2371=DERIVED_UNIT_ELEMENT(#5185,-3.);
#2372=DERIVED_UNIT_ELEMENT(#2378,1.);
#2373=DERIVED_UNIT_ELEMENT(#5185,-3.);
#2374=DERIVED_UNIT_ELEMENT(#2378,1.);
#2375=DERIVED_UNIT_ELEMENT(#5185,-3.);
#2376=DERIVED_UNIT_ELEMENT(#2378,1.);
#2377=DERIVED_UNIT_ELEMENT(#5185,-3.);
#2378=(
MASS_UNIT()
NAMED_UNIT(*)
SI_UNIT(.KILO.,.GRAM.)
);
#2379=DERIVED_UNIT((#2368,#2369));
#2380=DERIVED_UNIT((#2370,#2371));
#2381=DERIVED_UNIT((#2372,#2373));
#2382=DERIVED_UNIT((#2374,#2375));
#2383=DERIVED_UNIT((#2376,#2377));
#2384=MEASURE_REPRESENTATION_ITEM('density measure',
POSITIVE_RATIO_MEASURE(7850.),#2379);
#2385=MEASURE_REPRESENTATION_ITEM('density measure',
POSITIVE_RATIO_MEASURE(7850.),#2380);
#2386=MEASURE_REPRESENTATION_ITEM('density measure',
POSITIVE_RATIO_MEASURE(7850.),#2381);
#2387=MEASURE_REPRESENTATION_ITEM('density measure',
POSITIVE_RATIO_MEASURE(7850.),#2382);
#2388=MEASURE_REPRESENTATION_ITEM('density measure',
POSITIVE_RATIO_MEASURE(7850.),#2383);
#2389=PROPERTY_DEFINITION_REPRESENTATION(#2414,#2399);
#2390=PROPERTY_DEFINITION_REPRESENTATION(#2415,#2400);
#2391=PROPERTY_DEFINITION_REPRESENTATION(#2416,#2401);
#2392=PROPERTY_DEFINITION_REPRESENTATION(#2417,#2402);
#2393=PROPERTY_DEFINITION_REPRESENTATION(#2418,#2403);
#2394=PROPERTY_DEFINITION_REPRESENTATION(#2419,#2404);
#2395=PROPERTY_DEFINITION_REPRESENTATION(#2420,#2405);
#2396=PROPERTY_DEFINITION_REPRESENTATION(#2421,#2406);
#2397=PROPERTY_DEFINITION_REPRESENTATION(#2422,#2407);
#2398=PROPERTY_DEFINITION_REPRESENTATION(#2423,#2408);
#2399=REPRESENTATION('material name',(#2409),#5178);
#2400=REPRESENTATION('density',(#2384),#5178);
#2401=REPRESENTATION('material name',(#2410),#5179);
#2402=REPRESENTATION('density',(#2385),#5179);
#2403=REPRESENTATION('material name',(#2411),#5180);
#2404=REPRESENTATION('density',(#2386),#5180);
#2405=REPRESENTATION('material name',(#2412),#5181);
#2406=REPRESENTATION('density',(#2387),#5181);
#2407=REPRESENTATION('material name',(#2413),#5182);
#2408=REPRESENTATION('density',(#2388),#5182);
#2409=DESCRIPTIVE_REPRESENTATION_ITEM('Steel','Steel');
#2410=DESCRIPTIVE_REPRESENTATION_ITEM('Steel','Steel');
#2411=DESCRIPTIVE_REPRESENTATION_ITEM('Steel','Steel');
#2412=DESCRIPTIVE_REPRESENTATION_ITEM('Steel','Steel');
#2413=DESCRIPTIVE_REPRESENTATION_ITEM('Steel','Steel');
#2414=PROPERTY_DEFINITION('material property','material name',#5221);
#2415=PROPERTY_DEFINITION('material property','density of part',#5221);
#2416=PROPERTY_DEFINITION('material property','material name',#5222);
#2417=PROPERTY_DEFINITION('material property','density of part',#5222);
#2418=PROPERTY_DEFINITION('material property','material name',#5223);
#2419=PROPERTY_DEFINITION('material property','density of part',#5223);
#2420=PROPERTY_DEFINITION('material property','material name',#5224);
#2421=PROPERTY_DEFINITION('material property','density of part',#5224);
#2422=PROPERTY_DEFINITION('material property','material name',#5225);
#2423=PROPERTY_DEFINITION('material property','density of part',#5225);
#2424=AXIS2_PLACEMENT_3D('',#3336,#2678,#2679);
#2425=AXIS2_PLACEMENT_3D('',#3337,#2680,#2681);
#2426=AXIS2_PLACEMENT_3D('',#3338,#2682,#2683);
#2427=AXIS2_PLACEMENT_3D('',#3343,#2685,#2686);
#2428=AXIS2_PLACEMENT_3D('',#3346,#2688,#2689);
#2429=AXIS2_PLACEMENT_3D('',#3347,#2690,#2691);
#2430=AXIS2_PLACEMENT_3D('',#3352,#2693,#2694);
#2431=AXIS2_PLACEMENT_3D('',#3355,#2696,#2697);
#2432=AXIS2_PLACEMENT_3D('',#3356,#2698,#2699);
#2433=AXIS2_PLACEMENT_3D('',#3359,#2700,#2701);
#2434=AXIS2_PLACEMENT_3D('',#3363,#2703,#2704);
#2435=AXIS2_PLACEMENT_3D('',#3365,#2706,#2707);
#2436=AXIS2_PLACEMENT_3D('',#3418,#2710,#2711);
#2437=AXIS2_PLACEMENT_3D('',#3464,#2714,#2715);
#2438=AXIS2_PLACEMENT_3D('',#3510,#2718,#2719);
#2439=AXIS2_PLACEMENT_3D('',#3563,#2722,#2723);
#2440=AXIS2_PLACEMENT_3D('',#3566,#2724,#2725);
#2441=AXIS2_PLACEMENT_3D('',#3570,#2727,#2728);
#2442=AXIS2_PLACEMENT_3D('',#3572,#2730,#2731);
#2443=AXIS2_PLACEMENT_3D('',#3625,#2734,#2735);
#2444=AXIS2_PLACEMENT_3D('',#3671,#2738,#2739);
#2445=AXIS2_PLACEMENT_3D('',#3717,#2742,#2743);
#2446=AXIS2_PLACEMENT_3D('',#3770,#2746,#2747);
#2447=AXIS2_PLACEMENT_3D('',#3823,#2750,#2751);
#2448=AXIS2_PLACEMENT_3D('',#3869,#2754,#2755);
#2449=AXIS2_PLACEMENT_3D('',#3915,#2758,#2759);
#2450=AXIS2_PLACEMENT_3D('',#3968,#2762,#2763);
#2451=AXIS2_PLACEMENT_3D('',#3971,#2764,#2765);
#2452=AXIS2_PLACEMENT_3D('',#3975,#2767,#2768);
#2453=AXIS2_PLACEMENT_3D('',#3977,#2770,#2771);
#2454=AXIS2_PLACEMENT_3D('',#3982,#2773,#2774);
#2455=AXIS2_PLACEMENT_3D('',#3985,#2776,#2777);
#2456=AXIS2_PLACEMENT_3D('',#3986,#2778,#2779);
#2457=AXIS2_PLACEMENT_3D('',#3988,#2780,#2781);
#2458=AXIS2_PLACEMENT_3D('',#3992,#2783,#2784);
#2459=AXIS2_PLACEMENT_3D('',#3997,#2787,#2788);
#2460=AXIS2_PLACEMENT_3D('',#4002,#2791,#2792);
#2461=AXIS2_PLACEMENT_3D('',#4004,#2794,#2795);
#2462=AXIS2_PLACEMENT_3D('',#4006,#2796,#2797);
#2463=AXIS2_PLACEMENT_3D('',#4022,#2807,#2808);
#2464=AXIS2_PLACEMENT_3D('',#4024,#2810,#2811);
#2465=AXIS2_PLACEMENT_3D('',#4041,#2821,#2822);
#2466=AXIS2_PLACEMENT_3D('',#4042,#2823,#2824);
#2467=AXIS2_PLACEMENT_3D('',#4046,#2826,#2827);
#2468=AXIS2_PLACEMENT_3D('',#4051,#2830,#2831);
#2469=AXIS2_PLACEMENT_3D('',#4056,#2834,#2835);
#2470=AXIS2_PLACEMENT_3D('',#4058,#2837,#2838);
#2471=AXIS2_PLACEMENT_3D('',#4060,#2839,#2840);
#2472=AXIS2_PLACEMENT_3D('',#4062,#2841,#2842);
#2473=AXIS2_PLACEMENT_3D('',#4063,#2843,#2844);
#2474=AXIS2_PLACEMENT_3D('',#4087,#2848,#2849);
#2475=AXIS2_PLACEMENT_3D('',#4089,#2850,#2851);
#2476=AXIS2_PLACEMENT_3D('',#4091,#2852,#2853);
#2477=AXIS2_PLACEMENT_3D('',#4092,#2854,#2855);
#2478=AXIS2_PLACEMENT_3D('',#4094,#2857,#2858);
#2479=AXIS2_PLACEMENT_3D('',#4096,#2859,#2860);
#2480=AXIS2_PLACEMENT_3D('',#4098,#2861,#2862);
#2481=AXIS2_PLACEMENT_3D('',#4099,#2863,#2864);
#2482=AXIS2_PLACEMENT_3D('',#4101,#2866,#2867);
#2483=AXIS2_PLACEMENT_3D('',#4103,#2868,#2869);
#2484=AXIS2_PLACEMENT_3D('',#4105,#2870,#2871);
#2485=AXIS2_PLACEMENT_3D('',#4106,#2872,#2873);
#2486=AXIS2_PLACEMENT_3D('',#4108,#2875,#2876);
#2487=AXIS2_PLACEMENT_3D('',#4110,#2877,#2878);
#2488=AXIS2_PLACEMENT_3D('',#4112,#2879,#2880);
#2489=AXIS2_PLACEMENT_3D('',#4113,#2881,#2882);
#2490=AXIS2_PLACEMENT_3D('',#4115,#2884,#2885);
#2491=AXIS2_PLACEMENT_3D('',#4117,#2886,#2887);
#2492=AXIS2_PLACEMENT_3D('',#4119,#2888,#2889);
#2493=AXIS2_PLACEMENT_3D('',#4120,#2890,#2891);
#2494=AXIS2_PLACEMENT_3D('',#4122,#2893,#2894);
#2495=AXIS2_PLACEMENT_3D('',#4124,#2895,#2896);
#2496=AXIS2_PLACEMENT_3D('',#4126,#2897,#2898);
#2497=AXIS2_PLACEMENT_3D('',#4127,#2899,#2900);
#2498=AXIS2_PLACEMENT_3D('',#4129,#2902,#2903);
#2499=AXIS2_PLACEMENT_3D('',#4131,#2904,#2905);
#2500=AXIS2_PLACEMENT_3D('',#4661,#2907,#2908);
#2501=AXIS2_PLACEMENT_3D('',#4662,#2909,#2910);
#2502=AXIS2_PLACEMENT_3D('',#4664,#2911,#2912);
#2503=AXIS2_PLACEMENT_3D('',#4666,#2913,#2914);
#2504=AXIS2_PLACEMENT_3D('',#4667,#2915,#2916);
#2505=AXIS2_PLACEMENT_3D('',#4669,#2918,#2919);
#2506=AXIS2_PLACEMENT_3D('',#4671,#2921,#2922);
#2507=AXIS2_PLACEMENT_3D('',#4673,#2924,#2925);
#2508=AXIS2_PLACEMENT_3D('',#4675,#2927,#2928);
#2509=AXIS2_PLACEMENT_3D('',#4677,#2930,#2931);
#2510=AXIS2_PLACEMENT_3D('',#4679,#2932,#2933);
#2511=AXIS2_PLACEMENT_3D('',#4681,#2934,#2935);
#2512=AXIS2_PLACEMENT_3D('',#4682,#2936,#2937);
#2513=AXIS2_PLACEMENT_3D('',#4706,#2941,#2942);
#2514=AXIS2_PLACEMENT_3D('',#4708,#2943,#2944);
#2515=AXIS2_PLACEMENT_3D('',#4710,#2945,#2946);
#2516=AXIS2_PLACEMENT_3D('',#4711,#2947,#2948);
#2517=AXIS2_PLACEMENT_3D('',#4735,#2952,#2953);
#2518=AXIS2_PLACEMENT_3D('',#4737,#2954,#2955);
#2519=AXIS2_PLACEMENT_3D('',#4739,#2956,#2957);
#2520=AXIS2_PLACEMENT_3D('',#4740,#2958,#2959);
#2521=AXIS2_PLACEMENT_3D('',#4742,#2961,#2962);
#2522=AXIS2_PLACEMENT_3D('',#4744,#2963,#2964);
#2523=AXIS2_PLACEMENT_3D('',#4746,#2965,#2966);
#2524=AXIS2_PLACEMENT_3D('',#4747,#2967,#2968);
#2525=AXIS2_PLACEMENT_3D('',#4749,#2970,#2971);
#2526=AXIS2_PLACEMENT_3D('',#4751,#2972,#2973);
#2527=AXIS2_PLACEMENT_3D('',#4753,#2974,#2975);
#2528=AXIS2_PLACEMENT_3D('',#4754,#2976,#2977);
#2529=AXIS2_PLACEMENT_3D('',#4756,#2979,#2980);
#2530=AXIS2_PLACEMENT_3D('',#4758,#2981,#2982);
#2531=AXIS2_PLACEMENT_3D('',#4760,#2983,#2984);
#2532=AXIS2_PLACEMENT_3D('',#4761,#2985,#2986);
#2533=AXIS2_PLACEMENT_3D('',#4763,#2988,#2989);
#2534=AXIS2_PLACEMENT_3D('',#4765,#2990,#2991);
#2535=AXIS2_PLACEMENT_3D('',#4767,#2992,#2993);
#2536=AXIS2_PLACEMENT_3D('',#4768,#2994,#2995);
#2537=AXIS2_PLACEMENT_3D('',#4770,#2997,#2998);
#2538=AXIS2_PLACEMENT_3D('',#4772,#2999,#3000);
#2539=AXIS2_PLACEMENT_3D('',#4774,#3001,#3002);
#2540=AXIS2_PLACEMENT_3D('',#4775,#3003,#3004);
#2541=AXIS2_PLACEMENT_3D('',#4777,#3006,#3007);
#2542=AXIS2_PLACEMENT_3D('',#4780,#3009,#3010);
#2543=AXIS2_PLACEMENT_3D('',#4781,#3011,#3012);
#2544=AXIS2_PLACEMENT_3D('',#4784,#3014,#3015);
#2545=AXIS2_PLACEMENT_3D('',#4785,#3016,#3017);
#2546=AXIS2_PLACEMENT_3D('',#4788,#3019,#3020);
#2547=AXIS2_PLACEMENT_3D('',#4789,#3021,#3022);
#2548=AXIS2_PLACEMENT_3D('',#4792,#3024,#3025);
#2549=AXIS2_PLACEMENT_3D('',#4793,#3026,#3027);
#2550=AXIS2_PLACEMENT_3D('',#4796,#3029,#3030);
#2551=AXIS2_PLACEMENT_3D('',#4797,#3031,#3032);
#2552=AXIS2_PLACEMENT_3D('',#4800,#3034,#3035);
#2553=AXIS2_PLACEMENT_3D('',#4801,#3036,#3037);
#2554=AXIS2_PLACEMENT_3D('',#4804,#3039,#3040);
#2555=AXIS2_PLACEMENT_3D('',#4805,#3041,#3042);
#2556=AXIS2_PLACEMENT_3D('',#4808,#3044,#3045);
#2557=AXIS2_PLACEMENT_3D('',#4809,#3046,#3047);
#2558=AXIS2_PLACEMENT_3D('',#4811,#3048,#3049);
#2559=AXIS2_PLACEMENT_3D('',#4812,#3050,#3051);
#2560=AXIS2_PLACEMENT_3D('',#4814,#3053,#3054);
#2561=AXIS2_PLACEMENT_3D('',#4816,#3055,#3056);
#2562=AXIS2_PLACEMENT_3D('',#4817,#3057,#3058);
#2563=AXIS2_PLACEMENT_3D('',#4819,#3060,#3061);
#2564=AXIS2_PLACEMENT_3D('',#4821,#3062,#3063);
#2565=AXIS2_PLACEMENT_3D('',#4822,#3064,#3065);
#2566=AXIS2_PLACEMENT_3D('',#4824,#3067,#3068);
#2567=AXIS2_PLACEMENT_3D('',#4826,#3069,#3070);
#2568=AXIS2_PLACEMENT_3D('',#4827,#3071,#3072);
#2569=AXIS2_PLACEMENT_3D('',#4829,#3074,#3075);
#2570=AXIS2_PLACEMENT_3D('',#4831,#3076,#3077);
#2571=AXIS2_PLACEMENT_3D('',#4832,#3078,#3079);
#2572=AXIS2_PLACEMENT_3D('',#4834,#3081,#3082);
#2573=AXIS2_PLACEMENT_3D('',#4836,#3083,#3084);
#2574=AXIS2_PLACEMENT_3D('',#4837,#3085,#3086);
#2575=AXIS2_PLACEMENT_3D('',#4839,#3088,#3089);
#2576=AXIS2_PLACEMENT_3D('',#4841,#3090,#3091);
#2577=AXIS2_PLACEMENT_3D('',#4842,#3092,#3093);
#2578=AXIS2_PLACEMENT_3D('',#4844,#3095,#3096);
#2579=AXIS2_PLACEMENT_3D('',#4846,#3097,#3098);
#2580=AXIS2_PLACEMENT_3D('',#4847,#3099,#3100);
#2581=AXIS2_PLACEMENT_3D('',#4849,#3102,#3103);
#2582=AXIS2_PLACEMENT_3D('',#4851,#3105,#3106);
#2583=AXIS2_PLACEMENT_3D('',#4853,#3108,#3109);
#2584=AXIS2_PLACEMENT_3D('',#4857,#3112,#3113);
#2585=AXIS2_PLACEMENT_3D('',#4911,#3116,#3117);
#2586=AXIS2_PLACEMENT_3D('',#4912,#3118,#3119);
#2587=AXIS2_PLACEMENT_3D('',#4914,#3121,#3122);
#2588=AXIS2_PLACEMENT_3D('',#4916,#3124,#3125);
#2589=AXIS2_PLACEMENT_3D('',#4920,#3128,#3129);
#2590=AXIS2_PLACEMENT_3D('',#4974,#3132,#3133);
#2591=AXIS2_PLACEMENT_3D('',#4975,#3134,#3135);
#2592=AXIS2_PLACEMENT_3D('',#4977,#3137,#3138);
#2593=AXIS2_PLACEMENT_3D('',#4979,#3140,#3141);
#2594=AXIS2_PLACEMENT_3D('',#4983,#3144,#3145);
#2595=AXIS2_PLACEMENT_3D('',#5037,#3148,#3149);
#2596=AXIS2_PLACEMENT_3D('',#5038,#3150,#3151);
#2597=AXIS2_PLACEMENT_3D('',#5040,#3153,#3154);
#2598=AXIS2_PLACEMENT_3D('',#5042,#3156,#3157);
#2599=AXIS2_PLACEMENT_3D('',#5043,#3158,#3159);
#2600=AXIS2_PLACEMENT_3D('',#5045,#3161,#3162);
#2601=AXIS2_PLACEMENT_3D('',#5047,#3164,#3165);
#2602=AXIS2_PLACEMENT_3D('',#5048,#3166,#3167);
#2603=AXIS2_PLACEMENT_3D('',#5050,#3169,#3170);
#2604=AXIS2_PLACEMENT_3D('',#5052,#3172,#3173);
#2605=AXIS2_PLACEMENT_3D('',#5053,#3174,#3175);
#2606=AXIS2_PLACEMENT_3D('',#5054,#3176,#3177);
#2607=AXIS2_PLACEMENT_3D('',#5056,#3178,#3179);
#2608=AXIS2_PLACEMENT_3D('',#5059,#3181,#3182);
#2609=AXIS2_PLACEMENT_3D('',#5060,#3183,#3184);
#2610=AXIS2_PLACEMENT_3D('',#5062,#3185,#3186);
#2611=AXIS2_PLACEMENT_3D('',#5063,#3187,#3188);
#2612=AXIS2_PLACEMENT_3D('',#5065,#3189,#3190);
#2613=AXIS2_PLACEMENT_3D('',#5066,#3191,#3192);
#2614=AXIS2_PLACEMENT_3D('',#5068,#3193,#3194);
#2615=AXIS2_PLACEMENT_3D('',#5071,#3196,#3197);
#2616=AXIS2_PLACEMENT_3D('',#5072,#3198,#3199);
#2617=AXIS2_PLACEMENT_3D('',#5074,#3201,#3202);
#2618=AXIS2_PLACEMENT_3D('',#5076,#3203,#3204);
#2619=AXIS2_PLACEMENT_3D('',#5077,#3205,#3206);
#2620=AXIS2_PLACEMENT_3D('',#5079,#3208,#3209);
#2621=AXIS2_PLACEMENT_3D('',#5080,#3210,#3211);
#2622=AXIS2_PLACEMENT_3D('',#5082,#3212,#3213);
#2623=AXIS2_PLACEMENT_3D('',#5085,#3215,#3216);
#2624=AXIS2_PLACEMENT_3D('',#5086,#3217,#3218);
#2625=AXIS2_PLACEMENT_3D('',#5088,#3219,#3220);
#2626=AXIS2_PLACEMENT_3D('',#5089,#3221,#3222);
#2627=AXIS2_PLACEMENT_3D('',#5091,#3223,#3224);
#2628=AXIS2_PLACEMENT_3D('',#5092,#3225,#3226);
#2629=AXIS2_PLACEMENT_3D('',#5094,#3227,#3228);
#2630=AXIS2_PLACEMENT_3D('',#5097,#3230,#3231);
#2631=AXIS2_PLACEMENT_3D('',#5098,#3232,#3233);
#2632=AXIS2_PLACEMENT_3D('',#5100,#3235,#3236);
#2633=AXIS2_PLACEMENT_3D('',#5102,#3237,#3238);
#2634=AXIS2_PLACEMENT_3D('',#5103,#3239,#3240);
#2635=AXIS2_PLACEMENT_3D('',#5105,#3242,#3243);
#2636=AXIS2_PLACEMENT_3D('',#5106,#3244,#3245);
#2637=AXIS2_PLACEMENT_3D('',#5108,#3246,#3247);
#2638=AXIS2_PLACEMENT_3D('',#5111,#3249,#3250);
#2639=AXIS2_PLACEMENT_3D('',#5112,#3251,#3252);
#2640=AXIS2_PLACEMENT_3D('',#5114,#3253,#3254);
#2641=AXIS2_PLACEMENT_3D('',#5115,#3255,#3256);
#2642=AXIS2_PLACEMENT_3D('',#5117,#3257,#3258);
#2643=AXIS2_PLACEMENT_3D('',#5118,#3259,#3260);
#2644=AXIS2_PLACEMENT_3D('',#5120,#3261,#3262);
#2645=AXIS2_PLACEMENT_3D('',#5123,#3264,#3265);
#2646=AXIS2_PLACEMENT_3D('',#5124,#3266,#3267);
#2647=AXIS2_PLACEMENT_3D('',#5126,#3269,#3270);
#2648=AXIS2_PLACEMENT_3D('',#5128,#3271,#3272);
#2649=AXIS2_PLACEMENT_3D('',#5129,#3273,#3274);
#2650=AXIS2_PLACEMENT_3D('',#5131,#3276,#3277);
#2651=AXIS2_PLACEMENT_3D('',#5132,#3278,#3279);
#2652=AXIS2_PLACEMENT_3D('',#5134,#3280,#3281);
#2653=AXIS2_PLACEMENT_3D('',#5137,#3283,#3284);
#2654=AXIS2_PLACEMENT_3D('',#5138,#3285,#3286);
#2655=AXIS2_PLACEMENT_3D('',#5140,#3287,#3288);
#2656=AXIS2_PLACEMENT_3D('',#5141,#3289,#3290);
#2657=AXIS2_PLACEMENT_3D('',#5143,#3291,#3292);
#2658=AXIS2_PLACEMENT_3D('',#5144,#3293,#3294);
#2659=AXIS2_PLACEMENT_3D('',#5146,#3295,#3296);
#2660=AXIS2_PLACEMENT_3D('',#5149,#3298,#3299);
#2661=AXIS2_PLACEMENT_3D('',#5150,#3300,#3301);
#2662=AXIS2_PLACEMENT_3D('',#5152,#3303,#3304);
#2663=AXIS2_PLACEMENT_3D('',#5154,#3305,#3306);
#2664=AXIS2_PLACEMENT_3D('',#5155,#3307,#3308);
#2665=AXIS2_PLACEMENT_3D('',#5157,#3310,#3311);
#2666=AXIS2_PLACEMENT_3D('',#5158,#3312,#3313);
#2667=AXIS2_PLACEMENT_3D('',#5159,#3314,#3315);
#2668=AXIS2_PLACEMENT_3D('',#5160,#3316,#3317);
#2669=AXIS2_PLACEMENT_3D('',#5161,#3318,#3319);
#2670=AXIS2_PLACEMENT_3D('',#5162,#3320,#3321);
#2671=AXIS2_PLACEMENT_3D('',#5163,#3322,#3323);
#2672=AXIS2_PLACEMENT_3D('',#5164,#3324,#3325);
#2673=AXIS2_PLACEMENT_3D('',#5165,#3326,#3327);
#2674=AXIS2_PLACEMENT_3D('',#5166,#3328,#3329);
#2675=AXIS2_PLACEMENT_3D('',#5167,#3330,#3331);
#2676=AXIS2_PLACEMENT_3D('',#5168,#3332,#3333);
#2677=AXIS2_PLACEMENT_3D('',#5169,#3334,#3335);
#2678=DIRECTION('axis',(0.,0.,1.));
#2679=DIRECTION('refdir',(1.,0.,0.));
#2680=DIRECTION('axis',(0.,0.,1.));
#2681=DIRECTION('refdir',(1.,0.,0.));
#2682=DIRECTION('center_axis',(0.866025403784443,0.,0.499999999999992));
#2683=DIRECTION('ref_axis',(0.499999999999992,0.,-0.866025403784443));
#2684=DIRECTION('',(0.866025403784444,0.,0.499999999999991));
#2685=DIRECTION('center_axis',(-0.866025403784443,0.,-0.499999999999992));
#2686=DIRECTION('ref_axis',(-0.499999999999992,0.,0.866025403784443));
#2687=DIRECTION('',(0.866025403784443,0.,0.499999999999992));
#2688=DIRECTION('center_axis',(-0.866025403784443,0.,-0.499999999999992));
#2689=DIRECTION('ref_axis',(-0.499999999999992,0.,0.866025403784443));
#2690=DIRECTION('center_axis',(0.866025403784443,0.,0.499999999999992));
#2691=DIRECTION('ref_axis',(0.499999999999992,0.,-0.866025403784443));
#2692=DIRECTION('',(0.866025403784443,0.,0.499999999999993));
#2693=DIRECTION('center_axis',(-0.866025403784443,0.,-0.499999999999992));
#2694=DIRECTION('ref_axis',(-0.499999999999992,0.,0.866025403784443));
#2695=DIRECTION('',(0.866025403784443,0.,0.499999999999993));
#2696=DIRECTION('center_axis',(-0.866025403784443,0.,-0.499999999999992));
#2697=DIRECTION('ref_axis',(-0.499999999999992,0.,0.866025403784443));
#2698=DIRECTION('center_axis',(0.866025403784443,0.,0.499999999999992));
#2699=DIRECTION('ref_axis',(0.499999999999992,0.,-0.866025403784443));
#2700=DIRECTION('center_axis',(-0.866025403784443,0.,-0.499999999999992));
#2701=DIRECTION('ref_axis',(-0.499999999999992,0.,0.866025403784443));
#2702=DIRECTION('',(0.866025403784443,0.,0.499999999999992));
#2703=DIRECTION('center_axis',(-0.866025403784443,0.,-0.499999999999992));
#2704=DIRECTION('ref_axis',(-0.499999999999992,0.,0.866025403784443));
#2705=DIRECTION('',(0.866025403784443,0.,0.499999999999992));
#2706=DIRECTION('center_axis',(0.866025403784443,0.,0.499999999999992));
#2707=DIRECTION('ref_axis',(0.499999999999992,0.,-0.866025403784443));
#2708=DIRECTION('',(0.866025403784443,0.,0.499999999999992));
#2709=DIRECTION('',(0.866025403784443,0.,0.499999999999992));
#2710=DIRECTION('center_axis',(0.866025403784443,0.,0.499999999999992));
#2711=DIRECTION('ref_axis',(0.499999999999992,0.,-0.866025403784443));
#2712=DIRECTION('',(0.866025403784443,0.,0.499999999999992));
#2713=DIRECTION('',(0.866025403784443,0.,0.499999999999992));
#2714=DIRECTION('center_axis',(0.866025403784443,0.,0.499999999999992));
#2715=DIRECTION('ref_axis',(0.499999999999992,0.,-0.866025403784443));
#2716=DIRECTION('',(0.866025403784444,0.,0.499999999999991));
#2717=DIRECTION('',(0.866025403784443,0.,0.499999999999992));
#2718=DIRECTION('center_axis',(0.866025403784443,0.,0.499999999999992));
#2719=DIRECTION('ref_axis',(0.499999999999992,0.,-0.866025403784443));
#2720=DIRECTION('',(0.866025403784443,0.,0.499999999999993));
#2721=DIRECTION('',(0.866025403784443,0.,0.499999999999992));
#2722=DIRECTION('center_axis',(0.866025403784443,0.,0.499999999999992));
#2723=DIRECTION('ref_axis',(0.499999999999992,0.,-0.866025403784443));
#2724=DIRECTION('center_axis',(-0.866025403784443,0.,-0.499999999999992));
#2725=DIRECTION('ref_axis',(-0.499999999999992,0.,0.866025403784443));
#2726=DIRECTION('',(0.866025403784443,0.,0.499999999999992));
#2727=DIRECTION('center_axis',(-0.866025403784443,0.,-0.499999999999992));
#2728=DIRECTION('ref_axis',(-0.499999999999992,0.,0.866025403784443));
#2729=DIRECTION('',(0.866025403784443,0.,0.499999999999992));
#2730=DIRECTION('center_axis',(0.866025403784443,0.,0.499999999999992));
#2731=DIRECTION('ref_axis',(0.499999999999992,0.,-0.866025403784443));
#2732=DIRECTION('',(0.866025403784443,0.,0.499999999999992));
#2733=DIRECTION('',(0.866025403784443,0.,0.499999999999993));
#2734=DIRECTION('center_axis',(0.866025403784443,0.,0.499999999999992));
#2735=DIRECTION('ref_axis',(0.499999999999992,0.,-0.866025403784443));
#2736=DIRECTION('',(0.866025403784444,0.,0.499999999999991));
#2737=DIRECTION('',(0.866025403784443,0.,0.499999999999992));
#2738=DIRECTION('center_axis',(0.866025403784443,0.,0.499999999999992));
#2739=DIRECTION('ref_axis',(0.499999999999992,0.,-0.866025403784443));
#2740=DIRECTION('',(0.866025403784443,0.,0.499999999999992));
#2741=DIRECTION('',(0.866025403784443,0.,0.499999999999992));
#2742=DIRECTION('center_axis',(0.866025403784443,0.,0.499999999999992));
#2743=DIRECTION('ref_axis',(0.499999999999992,0.,-0.866025403784443));
#2744=DIRECTION('',(0.866025403784444,0.,0.49999999999999));
#2745=DIRECTION('',(0.866025403784441,0.,0.499999999999995));
#2746=DIRECTION('center_axis',(0.866025403784443,0.,0.499999999999992));
#2747=DIRECTION('ref_axis',(0.499999999999992,0.,-0.866025403784443));
#2748=DIRECTION('',(0.866025403784443,0.,0.499999999999993));
#2749=DIRECTION('',(0.866025403784443,0.,0.499999999999992));
#2750=DIRECTION('center_axis',(0.866025403784443,0.,0.499999999999992));
#2751=DIRECTION('ref_axis',(0.499999999999992,0.,-0.866025403784443));
#2752=DIRECTION('',(0.866025403784443,0.,0.499999999999992));
#2753=DIRECTION('',(0.866025403784443,0.,0.499999999999992));
#2754=DIRECTION('center_axis',(0.866025403784443,0.,0.499999999999992));
#2755=DIRECTION('ref_axis',(0.499999999999992,0.,-0.866025403784443));
#2756=DIRECTION('',(0.866025403784443,0.,0.499999999999992));
#2757=DIRECTION('',(0.866025403784443,0.,0.499999999999992));
#2758=DIRECTION('center_axis',(0.866025403784443,0.,0.499999999999992));
#2759=DIRECTION('ref_axis',(0.499999999999992,0.,-0.866025403784443));
#2760=DIRECTION('',(0.866025403784443,0.,0.499999999999992));
#2761=DIRECTION('',(0.866025403784444,0.,0.499999999999991));
#2762=DIRECTION('center_axis',(0.866025403784443,0.,0.499999999999992));
#2763=DIRECTION('ref_axis',(-0.433012701892211,0.500000000000004,0.750000000000002));
#2764=DIRECTION('center_axis',(-0.866025403784443,0.,-0.499999999999992));
#2765=DIRECTION('ref_axis',(-0.499999999999992,0.,0.866025403784443));
#2766=DIRECTION('',(0.866025403784443,0.,0.499999999999992));
#2767=DIRECTION('center_axis',(-0.866025403784443,0.,-0.499999999999992));
#2768=DIRECTION('ref_axis',(-0.499999999999992,0.,0.866025403784443));
#2769=DIRECTION('',(0.866025403784443,0.,0.499999999999992));
#2770=DIRECTION('center_axis',(0.866025403784443,0.,0.499999999999992));
#2771=DIRECTION('ref_axis',(-0.433012701892234,0.499999999999926,0.750000000000041));
#2772=DIRECTION('',(0.866025403784443,0.,0.499999999999992));
#2773=DIRECTION('center_axis',(-0.866025403784443,0.,-0.499999999999992));
#2774=DIRECTION('ref_axis',(-0.499999999999992,0.,0.866025403784443));
#2775=DIRECTION('',(0.866025403784442,0.,0.499999999999994));
#2776=DIRECTION('center_axis',(-0.866025403784443,0.,-0.499999999999992));
#2777=DIRECTION('ref_axis',(-0.499999999999992,0.,0.866025403784443));
#2778=DIRECTION('center_axis',(-0.866025403784443,0.,-0.499999999999992));
#2779=DIRECTION('ref_axis',(-0.499999999999992,0.,0.866025403784443));
#2780=DIRECTION('center_axis',(-0.866025403784443,0.,-0.499999999999992));
#2781=DIRECTION('ref_axis',(-0.499999999999992,0.,0.866025403784443));
#2782=DIRECTION('',(-0.433012701892229,-0.499999999999983,0.750000000000006));
#2783=DIRECTION('center_axis',(0.866025403784443,-2.25118642417821E-16,
0.499999999999992));
#2784=DIRECTION('ref_axis',(0.499999999999992,0.,-0.866025403784443));
#2785=DIRECTION('',(-0.433012701892221,-0.499999999999992,0.750000000000004));
#2786=DIRECTION('',(0.433012701892197,-0.500000000000028,-0.749999999999994));
#2787=DIRECTION('center_axis',(0.866025403784443,2.4704687096211E-16,0.499999999999992));
#2788=DIRECTION('ref_axis',(0.499999999999992,0.,-0.866025403784443));
#2789=DIRECTION('',(0.433012701892204,-0.500000000000004,-0.750000000000006));
#2790=DIRECTION('',(0.,1.,0.));
#2791=DIRECTION('center_axis',(0.866025403784443,0.,0.499999999999992));
#2792=DIRECTION('ref_axis',(0.499999999999992,0.,-0.866025403784443));
#2793=DIRECTION('',(0.,1.,0.));
#2794=DIRECTION('center_axis',(-0.866025403784443,0.,-0.499999999999992));
#2795=DIRECTION('ref_axis',(-0.499999999999992,0.,0.866025403784443));
#2796=DIRECTION('center_axis',(-0.866025403784443,0.,-0.499999999999992));
#2797=DIRECTION('ref_axis',(-0.499999999999992,0.,0.866025403784443));
#2798=DIRECTION('',(-0.43301270189221,0.500000000000002,0.750000000000004));
#2799=DIRECTION('',(0.25,0.866025403784439,-0.433012701892219));
#2800=DIRECTION('',(0.433012701892205,-0.500000000000012,-0.75));
#2801=DIRECTION('',(0.433012701892215,0.499999999999987,-0.750000000000011));
#2802=DIRECTION('',(0.25,-0.86602540378444,-0.433012701892216));
#2803=DIRECTION('',(-0.433012701892207,-0.499999999999993,0.750000000000012));
#2804=DIRECTION('',(0.,-1.,0.));
#2805=DIRECTION('',(-0.499999999999994,0.,0.866025403784442));
#2806=DIRECTION('',(0.,1.,0.));
#2807=DIRECTION('center_axis',(0.866025403784443,0.,0.499999999999992));
#2808=DIRECTION('ref_axis',(0.499999999999992,0.,-0.866025403784443));
#2809=DIRECTION('',(-0.866025403784443,0.,-0.499999999999992));
#2810=DIRECTION('center_axis',(-0.866025403784443,0.,-0.499999999999992));
#2811=DIRECTION('ref_axis',(-0.499999999999992,0.,0.866025403784443));
#2812=DIRECTION('',(0.433012701892209,-0.500000000000007,-0.750000000000001));
#2813=DIRECTION('',(0.250000000000001,0.866025403784442,-0.433012701892212));
#2814=DIRECTION('',(-0.433012701892215,0.499999999999997,0.750000000000005));
#2815=DIRECTION('',(0.,1.,0.));
#2816=DIRECTION('',(-0.499999999999994,0.,0.866025403784442));
#2817=DIRECTION('',(0.,-1.,0.));
#2818=DIRECTION('',(-0.433012701892214,-0.499999999999991,0.750000000000009));
#2819=DIRECTION('',(0.249999999999992,-0.866025403784442,-0.433012701892217));
#2820=DIRECTION('',(0.433012701892219,0.499999999999982,-0.750000000000012));
#2821=DIRECTION('center_axis',(0.866025403784443,0.,0.499999999999992));
#2822=DIRECTION('ref_axis',(0.499999999999992,0.,-0.866025403784443));
#2823=DIRECTION('center_axis',(-0.866025403784443,0.,-0.499999999999992));
#2824=DIRECTION('ref_axis',(-0.499999999999992,0.,0.866025403784443));
#2825=DIRECTION('',(-0.433012701892211,-0.49999999999998,0.750000000000018));
#2826=DIRECTION('center_axis',(-0.866025403784443,0.,-0.499999999999992));
#2827=DIRECTION('ref_axis',(-0.499999999999992,0.,0.866025403784443));
#2828=DIRECTION('',(0.433012701892242,0.49999999999998,-0.750000000000001));
#2829=DIRECTION('',(0.,1.,0.));
#2830=DIRECTION('center_axis',(-0.866025403784443,0.,-0.499999999999992));
#2831=DIRECTION('ref_axis',(-0.499999999999992,0.,0.866025403784443));
#2832=DIRECTION('',(0.,-1.,0.));
#2833=DIRECTION('',(0.433012701892204,-0.500000000000004,-0.750000000000006));
#2834=DIRECTION('center_axis',(-0.866025403784443,0.,-0.499999999999992));
#2835=DIRECTION('ref_axis',(-0.499999999999992,0.,0.866025403784443));
#2836=DIRECTION('',(-0.433012701892195,0.499999999999999,0.750000000000015));
#2837=DIRECTION('center_axis',(0.,-1.,0.));
#2838=DIRECTION('ref_axis',(0.,0.,-1.));
#2839=DIRECTION('center_axis',(0.,-1.,0.));
#2840=DIRECTION('ref_axis',(0.,0.,-1.));
#2841=DIRECTION('center_axis',(0.,1.,0.));
#2842=DIRECTION('ref_axis',(0.,0.,1.));
#2843=DIRECTION('center_axis',(0.,1.,0.));
#2844=DIRECTION('ref_axis',(0.,0.,1.));
#2845=DIRECTION('',(0.,-1.,0.));
#2846=DIRECTION('',(0.,1.,0.));
#2847=DIRECTION('',(0.,1.,0.));
#2848=DIRECTION('center_axis',(0.224143868042018,-0.965925826289067,0.129409522551263));
#2849=DIRECTION('ref_axis',(0.,-0.132788176096111,-0.991144439670156));
#2850=DIRECTION('center_axis',(0.224143868042018,-0.965925826289067,0.129409522551263));
#2851=DIRECTION('ref_axis',(0.974116947696296,0.22604462437946,0.));
#2852=DIRECTION('center_axis',(-0.224143868042018,0.965925826289067,-0.129409522551263));
#2853=DIRECTION('ref_axis',(-0.974116947696296,-0.22604462437946,0.));
#2854=DIRECTION('center_axis',(-0.224143868042018,0.965925826289067,-0.129409522551263));
#2855=DIRECTION('ref_axis',(-0.974116947696296,-0.22604462437946,0.));
#2856=DIRECTION('',(0.224143868042018,-0.965925826289067,0.129409522551263));
#2857=DIRECTION('center_axis',(0.433012701892223,-0.866025403784436,0.250000000000002));
#2858=DIRECTION('ref_axis',(0.5,0.,-0.866025403784439));
#2859=DIRECTION('center_axis',(0.433012701892223,-0.866025403784436,0.250000000000002));
#2860=DIRECTION('ref_axis',(0.894427190999914,0.447213595499962,0.));
#2861=DIRECTION('center_axis',(-0.433012701892223,0.866025403784436,-0.250000000000002));
#2862=DIRECTION('ref_axis',(-0.894427190999914,-0.447213595499962,0.));
#2863=DIRECTION('center_axis',(-0.433012701892223,0.866025403784436,-0.250000000000002));
#2864=DIRECTION('ref_axis',(-0.894427190999914,-0.447213595499962,0.));
#2865=DIRECTION('',(0.433012701892223,-0.866025403784437,0.250000000000002));
#2866=DIRECTION('center_axis',(0.612372435695796,-0.707106781186546,0.353553390593275));
#2867=DIRECTION('ref_axis',(0.5,0.,-0.866025403784438));
#2868=DIRECTION('center_axis',(0.612372435695796,-0.707106781186546,0.353553390593275));
#2869=DIRECTION('ref_axis',(0.755928946018453,0.654653670707979,0.));
#2870=DIRECTION('center_axis',(-0.612372435695796,0.707106781186546,-0.353553390593275));
#2871=DIRECTION('ref_axis',(-0.755928946018453,-0.654653670707979,0.));
#2872=DIRECTION('center_axis',(-0.612372435695796,0.707106781186546,-0.353553390593275));
#2873=DIRECTION('ref_axis',(-0.755928946018453,-0.654653670707979,0.));
#2874=DIRECTION('',(0.612372435695796,-0.707106781186546,0.353553390593275));
#2875=DIRECTION('center_axis',(0.,1.,0.));
#2876=DIRECTION('ref_axis',(0.,0.,1.));
#2877=DIRECTION('center_axis',(0.,1.,0.));
#2878=DIRECTION('ref_axis',(0.,0.,1.));
#2879=DIRECTION('center_axis',(0.,1.,0.));
#2880=DIRECTION('ref_axis',(0.,0.,1.));
#2881=DIRECTION('center_axis',(0.,1.,0.));
#2882=DIRECTION('ref_axis',(0.,0.,1.));
#2883=DIRECTION('',(0.,1.,0.));
#2884=DIRECTION('center_axis',(-0.224143868042018,0.965925826289067,-0.129409522551263));
#2885=DIRECTION('ref_axis',(0.,0.132788176096111,0.991144439670156));
#2886=DIRECTION('center_axis',(-0.224143868042018,0.965925826289067,-0.129409522551263));
#2887=DIRECTION('ref_axis',(-0.974116947696296,-0.22604462437946,0.));
#2888=DIRECTION('center_axis',(-0.224143868042018,0.965925826289067,-0.129409522551263));
#2889=DIRECTION('ref_axis',(-0.974116947696296,-0.22604462437946,0.));
#2890=DIRECTION('center_axis',(-0.224143868042018,0.965925826289067,-0.129409522551263));
#2891=DIRECTION('ref_axis',(-0.974116947696296,-0.22604462437946,0.));
#2892=DIRECTION('',(-0.224143868042018,0.965925826289067,-0.129409522551263));
#2893=DIRECTION('center_axis',(-0.433012701892223,0.866025403784436,-0.250000000000002));
#2894=DIRECTION('ref_axis',(-0.499999999999999,0.,0.866025403784439));
#2895=DIRECTION('center_axis',(-0.433012701892223,0.866025403784436,-0.250000000000002));
#2896=DIRECTION('ref_axis',(-0.894427190999914,-0.447213595499962,0.));
#2897=DIRECTION('center_axis',(-0.433012701892223,0.866025403784436,-0.250000000000002));
#2898=DIRECTION('ref_axis',(-0.894427190999914,-0.447213595499962,0.));
#2899=DIRECTION('center_axis',(-0.433012701892223,0.866025403784436,-0.250000000000002));
#2900=DIRECTION('ref_axis',(-0.894427190999914,-0.447213595499962,0.));
#2901=DIRECTION('',(-0.433012701892223,0.866025403784436,-0.250000000000002));
#2902=DIRECTION('center_axis',(0.866025403784443,0.,0.499999999999992));
#2903=DIRECTION('ref_axis',(0.499999999999992,0.,-0.866025403784443));
#2904=DIRECTION('center_axis',(-0.866025403784443,0.,-0.499999999999992));
#2905=DIRECTION('ref_axis',(-0.499999999999992,0.,0.866025403784443));
#2906=DIRECTION('',(0.866025403784443,0.,0.499999999999992));
#2907=DIRECTION('center_axis',(-0.866025403784443,0.,-0.499999999999992));
#2908=DIRECTION('ref_axis',(-0.499999999999992,0.,0.866025403784443));
#2909=DIRECTION('center_axis',(-0.612372435695796,0.707106781186546,-0.353553390593275));
#2910=DIRECTION('ref_axis',(-0.5,0.,0.866025403784438));
#2911=DIRECTION('center_axis',(-0.612372435695796,0.707106781186546,-0.353553390593275));
#2912=DIRECTION('ref_axis',(-0.755928946018453,-0.654653670707979,0.));
#2913=DIRECTION('center_axis',(-0.612372435695796,0.707106781186546,-0.353553390593275));
#2914=DIRECTION('ref_axis',(-0.755928946018453,-0.654653670707979,0.));
#2915=DIRECTION('center_axis',(-0.612372435695796,0.707106781186546,-0.353553390593275));
#2916=DIRECTION('ref_axis',(-0.755928946018453,-0.654653670707979,0.));
#2917=DIRECTION('',(-0.612372435695796,0.707106781186546,-0.353553390593275));
#2918=DIRECTION('center_axis',(0.,1.,0.));
#2919=DIRECTION('ref_axis',(0.,0.,1.));
#2920=DIRECTION('',(0.,1.,0.));
#2921=DIRECTION('center_axis',(-0.224143868042018,0.965925826289067,-0.129409522551263));
#2922=DIRECTION('ref_axis',(-0.974116947696296,-0.22604462437946,0.));
#2923=DIRECTION('',(-0.224143868042018,0.965925826289067,-0.129409522551263));
#2924=DIRECTION('center_axis',(-0.433012701892223,0.866025403784437,-0.250000000000002));
#2925=DIRECTION('ref_axis',(-0.894427190999914,-0.447213595499962,0.));
#2926=DIRECTION('',(-0.433012701892223,0.866025403784436,-0.250000000000002));
#2927=DIRECTION('center_axis',(-0.612372435695796,0.707106781186546,-0.353553390593275));
#2928=DIRECTION('ref_axis',(-0.755928946018453,-0.654653670707979,0.));
#2929=DIRECTION('',(-0.612372435695796,0.707106781186546,-0.353553390593275));
#2930=DIRECTION('center_axis',(0.433012701892215,0.499999999999992,-0.750000000000008));
#2931=DIRECTION('ref_axis',(-0.866025403784443,0.,-0.499999999999992));
#2932=DIRECTION('center_axis',(0.433012701892215,0.499999999999992,-0.750000000000008));
#2933=DIRECTION('ref_axis',(-0.649519052838319,0.750000000000008,0.125000000000006));
#2934=DIRECTION('center_axis',(-0.433012701892215,-0.499999999999992,0.750000000000008));
#2935=DIRECTION('ref_axis',(0.649519052838319,-0.750000000000008,-0.125000000000006));
#2936=DIRECTION('center_axis',(-0.433012701892215,-0.499999999999992,0.750000000000008));
#2937=DIRECTION('ref_axis',(0.649519052838319,-0.750000000000008,-0.125000000000006));
#2938=DIRECTION('',(0.433012701892215,0.499999999999992,-0.750000000000008));
#2939=DIRECTION('',(-0.433012701892199,-0.500000000000005,0.750000000000008));
#2940=DIRECTION('',(-0.433012701892214,-0.499999999999978,0.750000000000018));
#2941=DIRECTION('center_axis',(-0.433012701892211,0.500000000000004,0.750000000000002));
#2942=DIRECTION('ref_axis',(0.866025403784443,0.,0.499999999999992));
#2943=DIRECTION('center_axis',(-0.433012701892211,0.500000000000004,0.750000000000002));
#2944=DIRECTION('ref_axis',(-0.649519052838324,-0.750000000000002,0.125000000000015));
#2945=DIRECTION('center_axis',(0.433012701892211,-0.500000000000004,-0.750000000000002));
#2946=DIRECTION('ref_axis',(0.649519052838324,0.750000000000002,-0.125000000000015));
#2947=DIRECTION('center_axis',(0.433012701892211,-0.500000000000004,-0.750000000000002));
#2948=DIRECTION('ref_axis',(0.649519052838324,0.750000000000002,-0.125000000000015));
#2949=DIRECTION('',(-0.433012701892211,0.500000000000004,0.750000000000002));
#2950=DIRECTION('',(0.433012701892208,-0.499999999999987,-0.750000000000015));
#2951=DIRECTION('',(0.433012701892233,-0.50000000000002,-0.749999999999979));
#2952=DIRECTION('center_axis',(0.642402019910919,0.482962913144524,-0.595034847165548));
#2953=DIRECTION('ref_axis',(-0.679542161318994,0.,-0.733636456966194));
#2954=DIRECTION('center_axis',(0.642402019910919,0.482962913144524,-0.595034847165548));
#2955=DIRECTION('ref_axis',(0.510942898759438,0.308782699291242,0.802240985506049));
#2956=DIRECTION('center_axis',(-0.642402019910919,-0.482962913144524,0.595034847165548));
#2957=DIRECTION('ref_axis',(-0.510942898759438,-0.308782699291242,-0.802240985506049));
#2958=DIRECTION('center_axis',(-0.642402019910919,-0.482962913144524,0.595034847165548));
#2959=DIRECTION('ref_axis',(-0.510942898759438,-0.308782699291242,-0.802240985506049));
#2960=DIRECTION('',(0.642402019910919,0.482962913144524,-0.595034847165548));
#2961=DIRECTION('center_axis',(-0.194114283826876,0.482962913144539,0.853853892268062));
#2962=DIRECTION('ref_axis',(0.975118889534635,0.,0.221682546161714));
#2963=DIRECTION('center_axis',(-0.194114283826876,0.482962913144539,0.853853892268062));
#2964=DIRECTION('ref_axis',(0.706703285860956,-0.534827323670698,0.463174048936862));
#2965=DIRECTION('center_axis',(0.194114283826876,-0.482962913144539,-0.853853892268062));
#2966=DIRECTION('ref_axis',(-0.706703285860956,0.534827323670698,-0.463174048936862));
#2967=DIRECTION('center_axis',(0.194114283826876,-0.482962913144539,-0.853853892268062));
#2968=DIRECTION('ref_axis',(-0.706703285860956,0.534827323670698,-0.463174048936862));
#2969=DIRECTION('',(-0.194114283826876,0.482962913144539,0.853853892268062));
#2970=DIRECTION('center_axis',(0.808012701892221,0.433012701892207,-0.399519052838338));
#2971=DIRECTION('ref_axis',(-0.443226594010285,0.,-0.89640960858418));
#2972=DIRECTION('center_axis',(0.808012701892221,0.433012701892207,-0.399519052838338));
#2973=DIRECTION('ref_axis',(0.365367827064589,0.163691536870759,0.916357698556077));
#2974=DIRECTION('center_axis',(-0.808012701892221,-0.433012701892208,0.399519052838338));
#2975=DIRECTION('ref_axis',(-0.365367827064589,-0.163691536870759,-0.916357698556077));
#2976=DIRECTION('center_axis',(-0.808012701892221,-0.433012701892207,0.399519052838338));
#2977=DIRECTION('ref_axis',(-0.365367827064589,-0.163691536870759,-0.916357698556077));
#2978=DIRECTION('',(0.808012701892221,0.433012701892207,-0.399519052838338));
#2979=DIRECTION('center_axis',(0.058012701892234,0.433012701892226,0.899519052838325));
#2980=DIRECTION('ref_axis',(0.997926790235505,0.,-0.064359314246356));
#2981=DIRECTION('center_axis',(0.058012701892234,0.433012701892226,0.899519052838325));
#2982=DIRECTION('ref_axis',(0.752666161685325,-0.610905132370716,0.245537305306135));
#2983=DIRECTION('center_axis',(-0.0580127018922341,-0.433012701892225,-0.899519052838325));
#2984=DIRECTION('ref_axis',(-0.752666161685325,0.610905132370716,-0.245537305306135));
#2985=DIRECTION('center_axis',(-0.058012701892234,-0.433012701892226,-0.899519052838325));
#2986=DIRECTION('ref_axis',(-0.752666161685325,0.610905132370716,-0.245537305306135));
#2987=DIRECTION('',(0.058012701892234,0.433012701892226,0.899519052838325));
#2988=DIRECTION('center_axis',(0.918558653543694,0.353553390593261,-0.176776695296649));
#2989=DIRECTION('ref_axis',(-0.188982236504625,0.,-0.981980506061963));
#2990=DIRECTION('center_axis',(0.918558653543694,0.353553390593261,-0.176776695296649));
#2991=DIRECTION('ref_axis',(0.188982236504626,0.,0.981980506061964));
#2992=DIRECTION('center_axis',(-0.918558653543694,-0.353553390593261,0.176776695296649));
#2993=DIRECTION('ref_axis',(-0.188982236504626,-5.55111512312578E-17,-0.981980506061963));
#2994=DIRECTION('center_axis',(-0.918558653543694,-0.353553390593261,0.176776695296649));
#2995=DIRECTION('ref_axis',(-0.188982236504626,0.,-0.981980506061964));
#2996=DIRECTION('',(0.918558653543694,0.353553390593261,-0.176776695296649));
#2997=DIRECTION('center_axis',(0.30618621784791,0.353553390593282,0.883883476483177));
#2998=DIRECTION('ref_axis',(0.944911182523063,0.,-0.327326835354004));
#2999=DIRECTION('center_axis',(0.30618621784791,0.353553390593282,0.883883476483177));
#3000=DIRECTION('ref_axis',(0.755928946018457,-0.654653670707974,-7.66053886991358E-15));
#3001=DIRECTION('center_axis',(-0.30618621784791,-0.353553390593282,-0.883883476483177));
#3002=DIRECTION('ref_axis',(-0.755928946018457,0.654653670707974,7.60502771868232E-15));
#3003=DIRECTION('center_axis',(-0.30618621784791,-0.353553390593282,-0.883883476483177));
#3004=DIRECTION('ref_axis',(-0.755928946018457,0.654653670707974,7.66053886991358E-15));
#3005=DIRECTION('',(0.30618621784791,0.353553390593282,0.883883476483177));
#3006=DIRECTION('center_axis',(0.433012701892215,-0.499999999999992,-0.750000000000008));
#3007=DIRECTION('ref_axis',(0.649519052838319,0.750000000000008,-0.125000000000006));
#3008=DIRECTION('',(0.433012701892215,-0.499999999999992,-0.750000000000008));
#3009=DIRECTION('center_axis',(0.433012701892211,-0.500000000000004,-0.750000000000002));
#3010=DIRECTION('ref_axis',(0.,0.832050294337842,-0.554700196225231));
#3011=DIRECTION('center_axis',(-0.433012701892211,-0.500000000000004,0.750000000000002));
#3012=DIRECTION('ref_axis',(0.649519052838324,-0.750000000000002,-0.125000000000015));
#3013=DIRECTION('',(-0.433012701892211,-0.500000000000004,0.750000000000002));
#3014=DIRECTION('center_axis',(-0.433012701892215,-0.499999999999992,0.750000000000008));
#3015=DIRECTION('ref_axis',(0.,-0.832050294337851,-0.554700196225219));
#3016=DIRECTION('center_axis',(0.194114283826879,-0.482962913144528,-0.853853892268068));
#3017=DIRECTION('ref_axis',(-0.70670328586096,0.534827323670699,-0.463174048936855));
#3018=DIRECTION('',(0.194114283826879,-0.482962913144527,-0.853853892268068));
#3019=DIRECTION('center_axis',(0.194114283826876,-0.482962913144539,-0.853853892268062));
#3020=DIRECTION('ref_axis',(0.,0.87041002959648,-0.492327513326093));
#3021=DIRECTION('center_axis',(-0.642402019910915,-0.482962913144535,0.595034847165542));
#3022=DIRECTION('ref_axis',(-0.510942898759436,-0.308782699291236,-0.802240985506053));
#3023=DIRECTION('',(-0.642402019910915,-0.482962913144535,0.595034847165542));
#3024=DIRECTION('center_axis',(-0.642402019910919,-0.482962913144524,0.595034847165548));
#3025=DIRECTION('ref_axis',(0.679542161318994,0.,0.733636456966194));
#3026=DIRECTION('center_axis',(-0.0580127018922311,-0.433012701892215,-0.89951905283833));
#3027=DIRECTION('ref_axis',(-0.752666161685329,0.610905132370714,-0.245537305306127));
#3028=DIRECTION('',(-0.0580127018922311,-0.433012701892215,-0.89951905283833));
#3029=DIRECTION('center_axis',(-0.0580127018922341,-0.433012701892225,-0.899519052838325));
#3030=DIRECTION('ref_axis',(0.,0.901036538010451,-0.433743192649915));
#3031=DIRECTION('center_axis',(-0.808012701892218,-0.433012701892218,0.399519052838333));
#3032=DIRECTION('ref_axis',(-0.365367827064587,-0.163691536870751,-0.916357698556079));
#3033=DIRECTION('',(-0.808012701892218,-0.433012701892218,0.399519052838333));
#3034=DIRECTION('center_axis',(-0.808012701892221,-0.433012701892208,0.399519052838338));
#3035=DIRECTION('ref_axis',(0.472347490483135,-0.881412416655384,0.));
#3036=DIRECTION('center_axis',(-0.306186217847908,-0.353553390593273,-0.883883476483181));
#3037=DIRECTION('ref_axis',(-0.755928946018462,0.654653670707968,1.58761892521397E-14));
#3038=DIRECTION('',(-0.306186217847908,-0.353553390593273,-0.883883476483181));
#3039=DIRECTION('center_axis',(-0.30618621784791,-0.353553390593282,-0.883883476483177));
#3040=DIRECTION('ref_axis',(0.,0.928476690885255,-0.371390676354114));
#3041=DIRECTION('center_axis',(-0.918558653543692,-0.35355339059327,0.176776695296645));
#3042=DIRECTION('ref_axis',(-0.188982236504625,1.0547118733939E-14,-0.981980506061964));
#3043=DIRECTION('',(-0.918558653543692,-0.35355339059327,0.176776695296645));
#3044=DIRECTION('center_axis',(-0.918558653543694,-0.353553390593261,0.176776695296649));
#3045=DIRECTION('ref_axis',(0.359210604053538,-0.933256525257387,0.));
#3046=DIRECTION('center_axis',(-0.433012701892215,-0.499999999999992,0.750000000000008));
#3047=DIRECTION('ref_axis',(0.866025403784443,0.,0.499999999999992));
#3048=DIRECTION('center_axis',(-0.433012701892215,-0.499999999999992,0.750000000000008));
#3049=DIRECTION('ref_axis',(0.649519052838319,-0.750000000000008,-0.125000000000006));
#3050=DIRECTION('center_axis',(-0.433012701892215,-0.499999999999992,0.750000000000008));
#3051=DIRECTION('ref_axis',(0.649519052838319,-0.750000000000008,-0.125000000000006));
#3052=DIRECTION('',(-0.433012701892215,-0.499999999999992,0.750000000000008));
#3053=DIRECTION('center_axis',(0.433012701892211,-0.500000000000004,-0.750000000000002));
#3054=DIRECTION('ref_axis',(-0.866025403784443,0.,-0.499999999999992));
#3055=DIRECTION('center_axis',(0.433012701892211,-0.500000000000004,-0.750000000000002));
#3056=DIRECTION('ref_axis',(0.649519052838324,0.750000000000002,-0.125000000000015));
#3057=DIRECTION('center_axis',(0.433012701892211,-0.500000000000004,-0.750000000000002));
#3058=DIRECTION('ref_axis',(0.649519052838324,0.750000000000002,-0.125000000000015));
#3059=DIRECTION('',(0.433012701892211,-0.500000000000004,-0.750000000000002));
#3060=DIRECTION('center_axis',(-0.642402019910919,-0.482962913144524,0.595034847165548));
#3061=DIRECTION('ref_axis',(0.679542161318994,0.,0.733636456966194));
#3062=DIRECTION('center_axis',(-0.642402019910919,-0.482962913144524,0.595034847165548));
#3063=DIRECTION('ref_axis',(-0.510942898759438,-0.308782699291242,-0.802240985506049));
#3064=DIRECTION('center_axis',(-0.642402019910919,-0.482962913144524,0.595034847165548));
#3065=DIRECTION('ref_axis',(-0.510942898759438,-0.308782699291242,-0.802240985506049));
#3066=DIRECTION('',(-0.642402019910919,-0.482962913144524,0.595034847165548));
#3067=DIRECTION('center_axis',(0.194114283826876,-0.482962913144539,-0.853853892268062));
#3068=DIRECTION('ref_axis',(-0.975118889534635,0.,-0.221682546161714));
#3069=DIRECTION('center_axis',(0.194114283826876,-0.482962913144539,-0.853853892268062));
#3070=DIRECTION('ref_axis',(-0.706703285860956,0.534827323670698,-0.463174048936862));
#3071=DIRECTION('center_axis',(0.194114283826876,-0.482962913144539,-0.853853892268062));
#3072=DIRECTION('ref_axis',(-0.706703285860956,0.534827323670698,-0.463174048936862));
#3073=DIRECTION('',(0.194114283826876,-0.482962913144539,-0.853853892268062));
#3074=DIRECTION('center_axis',(-0.808012701892221,-0.433012701892208,0.399519052838338));
#3075=DIRECTION('ref_axis',(0.443226594010285,0.,0.89640960858418));
#3076=DIRECTION('center_axis',(-0.808012701892221,-0.433012701892208,0.399519052838338));
#3077=DIRECTION('ref_axis',(-0.365367827064589,-0.163691536870759,-0.916357698556077));
#3078=DIRECTION('center_axis',(-0.808012701892221,-0.433012701892207,0.399519052838338));
#3079=DIRECTION('ref_axis',(-0.365367827064589,-0.163691536870759,-0.916357698556077));
#3080=DIRECTION('',(-0.808012701892221,-0.433012701892207,0.399519052838338));
#3081=DIRECTION('center_axis',(-0.0580127018922341,-0.433012701892225,-0.899519052838325));
#3082=DIRECTION('ref_axis',(-0.997926790235505,0.,0.0643593142463562));
#3083=DIRECTION('center_axis',(-0.0580127018922341,-0.433012701892225,-0.899519052838325));
#3084=DIRECTION('ref_axis',(-0.752666161685325,0.610905132370716,-0.245537305306135));
#3085=DIRECTION('center_axis',(-0.0580127018922342,-0.433012701892225,-0.899519052838325));
#3086=DIRECTION('ref_axis',(-0.752666161685325,0.610905132370716,-0.245537305306135));
#3087=DIRECTION('',(-0.0580127018922342,-0.433012701892225,-0.899519052838325));
#3088=DIRECTION('center_axis',(-0.918558653543694,-0.353553390593261,0.176776695296649));
#3089=DIRECTION('ref_axis',(0.188982236504625,0.,0.981980506061963));
#3090=DIRECTION('center_axis',(-0.918558653543694,-0.353553390593261,0.176776695296649));
#3091=DIRECTION('ref_axis',(-0.188982236504626,-5.55111512312578E-17,-0.981980506061963));
#3092=DIRECTION('center_axis',(-0.918558653543694,-0.353553390593261,0.176776695296649));
#3093=DIRECTION('ref_axis',(-0.188982236504626,0.,-0.981980506061963));
#3094=DIRECTION('',(-0.918558653543694,-0.353553390593261,0.176776695296649));
#3095=DIRECTION('center_axis',(-0.30618621784791,-0.353553390593282,-0.883883476483177));
#3096=DIRECTION('ref_axis',(-0.944911182523063,0.,0.327326835354004));
#3097=DIRECTION('center_axis',(-0.30618621784791,-0.353553390593282,-0.883883476483177));
#3098=DIRECTION('ref_axis',(-0.755928946018457,0.654653670707974,7.60502771868232E-15));
#3099=DIRECTION('center_axis',(-0.306186217847911,-0.353553390593282,-0.883883476483177));
#3100=DIRECTION('ref_axis',(-0.755928946018457,0.654653670707974,7.66053886991358E-15));
#3101=DIRECTION('',(-0.30618621784791,-0.353553390593282,-0.883883476483177));
#3102=DIRECTION('center_axis',(-0.499999999999992,0.,0.866025403784443));
#3103=DIRECTION('ref_axis',(0.866025403784443,0.,0.499999999999992));
#3104=DIRECTION('',(0.866025403784443,0.,0.499999999999992));
#3105=DIRECTION('center_axis',(0.499999999999992,0.,-0.866025403784443));
#3106=DIRECTION('ref_axis',(-0.866025403784443,0.,-0.499999999999992));
#3107=DIRECTION('',(0.866025403784443,0.,0.499999999999992));
#3108=DIRECTION('center_axis',(-0.499999999999999,0.,0.866025403784439));
#3109=DIRECTION('ref_axis',(0.866025403784439,0.,0.499999999999999));
#3110=DIRECTION('',(0.,1.,0.));
#3111=DIRECTION('',(0.866025403784443,0.,0.499999999999992));
#3112=DIRECTION('center_axis',(0.499999999999999,0.,-0.866025403784439));
#3113=DIRECTION('ref_axis',(-0.866025403784439,0.,-0.499999999999999));
#3114=DIRECTION('',(0.866025403784443,0.,0.499999999999992));
#3115=DIRECTION('',(0.,1.,0.));
#3116=DIRECTION('center_axis',(0.866025403784443,0.,0.499999999999992));
#3117=DIRECTION('ref_axis',(0.499999999999992,0.,-0.866025403784443));
#3118=DIRECTION('center_axis',(0.249999999999998,0.866025403784436,-0.433012701892225));
#3119=DIRECTION('ref_axis',(-0.866025403784443,0.,-0.499999999999992));
#3120=DIRECTION('',(0.866025403784443,0.,0.499999999999992));
#3121=DIRECTION('center_axis',(-0.249999999999998,-0.866025403784436,0.433012701892225));
#3122=DIRECTION('ref_axis',(0.866025403784444,0.,0.499999999999991));
#3123=DIRECTION('',(0.866025403784443,0.,0.499999999999992));
#3124=DIRECTION('center_axis',(0.249999999999991,0.866025403784436,-0.433012701892229));
#3125=DIRECTION('ref_axis',(-0.866025403784452,0.,-0.499999999999977));
#3126=DIRECTION('',(0.433012701892214,-0.500000000000001,-0.750000000000002));
#3127=DIRECTION('',(0.866025403784443,0.,0.499999999999992));
#3128=DIRECTION('center_axis',(-0.249999999999991,-0.866025403784436,0.433012701892229));
#3129=DIRECTION('ref_axis',(0.866025403784451,0.,0.499999999999978));
#3130=DIRECTION('',(0.866025403784443,0.,0.499999999999992));
#3131=DIRECTION('',(0.433012701892241,-0.499999999999971,-0.750000000000007));
#3132=DIRECTION('center_axis',(0.866025403784443,0.,0.499999999999992));
#3133=DIRECTION('ref_axis',(0.499999999999992,0.,-0.866025403784443));
#3134=DIRECTION('center_axis',(0.249999999999992,-0.866025403784443,-0.433012701892215));
#3135=DIRECTION('ref_axis',(0.,0.447213595499952,-0.894427190999919));
#3136=DIRECTION('',(0.866025403784443,0.,0.499999999999992));
#3137=DIRECTION('center_axis',(-0.249999999999991,0.866025403784443,0.433012701892215));
#3138=DIRECTION('ref_axis',(0.,-0.447213595499952,0.894427190999919));
#3139=DIRECTION('',(0.866025403784443,0.,0.499999999999992));
#3140=DIRECTION('center_axis',(0.249999999999984,-0.866025403784443,-0.433012701892219));
#3141=DIRECTION('ref_axis',(0.,0.447213595499956,-0.894427190999917));
#3142=DIRECTION('',(-0.433012701892197,-0.499999999999982,0.750000000000025));
#3143=DIRECTION('',(0.866025403784443,0.,0.499999999999992));
#3144=DIRECTION('center_axis',(-0.249999999999985,0.866025403784443,0.433012701892219));
#3145=DIRECTION('ref_axis',(0.,-0.447213595499956,0.894427190999917));
#3146=DIRECTION('',(0.866025403784443,0.,0.499999999999992));
#3147=DIRECTION('',(-0.433012701892228,-0.49999999999999,0.750000000000002));
#3148=DIRECTION('center_axis',(0.866025403784443,0.,0.499999999999992));
#3149=DIRECTION('ref_axis',(0.499999999999992,0.,-0.866025403784443));
#3150=DIRECTION('center_axis',(-0.499999999999992,0.,0.866025403784443));
#3151=DIRECTION('ref_axis',(0.866025403784443,0.,0.499999999999992));
#3152=DIRECTION('',(0.866025403784442,0.,0.499999999999994));
#3153=DIRECTION('center_axis',(0.499999999999992,0.,-0.866025403784443));
#3154=DIRECTION('ref_axis',(-0.866025403784443,0.,-0.499999999999992));
#3155=DIRECTION('',(0.866025403784443,0.,0.499999999999992));
#3156=DIRECTION('center_axis',(0.,1.,0.));
#3157=DIRECTION('ref_axis',(0.,0.,1.));
#3158=DIRECTION('center_axis',(0.249999999999992,-0.866025403784443,-0.433012701892215));
#3159=DIRECTION('ref_axis',(0.,0.447213595499952,-0.894427190999919));
#3160=DIRECTION('',(0.866025403784443,0.,0.499999999999992));
#3161=DIRECTION('center_axis',(-0.249999999999992,0.866025403784443,0.433012701892215));
#3162=DIRECTION('ref_axis',(0.,-0.447213595499952,0.894427190999919));
#3163=DIRECTION('',(0.866025403784444,0.,0.499999999999991));
#3164=DIRECTION('center_axis',(-0.433012701892215,-0.499999999999992,0.750000000000008));
#3165=DIRECTION('ref_axis',(0.866025403784443,0.,0.499999999999992));
#3166=DIRECTION('center_axis',(0.249999999999998,0.866025403784436,-0.433012701892225));
#3167=DIRECTION('ref_axis',(-0.866025403784443,0.,-0.499999999999992));
#3168=DIRECTION('',(0.866025403784442,0.,0.499999999999994));
#3169=DIRECTION('center_axis',(-0.249999999999998,-0.866025403784436,0.433012701892225));
#3170=DIRECTION('ref_axis',(0.866025403784443,0.,0.499999999999992));
#3171=DIRECTION('',(0.866025403784442,0.,0.499999999999994));
#3172=DIRECTION('center_axis',(0.433012701892211,-0.500000000000004,-0.750000000000002));
#3173=DIRECTION('ref_axis',(-0.866025403784443,0.,-0.499999999999992));
#3174=DIRECTION('axis',(0.,0.,1.));
#3175=DIRECTION('refdir',(1.,0.,0.));
#3176=DIRECTION('center_axis',(-0.612372435695796,0.707106781186546,-0.353553390593275));
#3177=DIRECTION('ref_axis',(-0.755928946018453,-0.654653670707979,0.));
#3178=DIRECTION('center_axis',(0.612372435695796,-0.707106781186546,0.353553390593275));
#3179=DIRECTION('ref_axis',(0.755928946018453,0.654653670707979,0.));
#3180=DIRECTION('',(0.612372435695796,-0.707106781186546,0.353553390593275));
#3181=DIRECTION('center_axis',(0.612372435695796,-0.707106781186546,0.353553390593275));
#3182=DIRECTION('ref_axis',(0.755928946018453,0.654653670707979,0.));
#3183=DIRECTION('center_axis',(0.612372435695796,-0.707106781186546,0.353553390593275));
#3184=DIRECTION('ref_axis',(0.5,0.,-0.866025403784438));
#3185=DIRECTION('center_axis',(0.612372435695796,-0.707106781186546,0.353553390593275));
#3186=DIRECTION('ref_axis',(0.755928946018453,0.654653670707979,0.));
#3187=DIRECTION('center_axis',(0.612372435695796,-0.707106781186546,0.353553390593275));
#3188=DIRECTION('ref_axis',(0.5,0.,-0.866025403784438));
#3189=DIRECTION('center_axis',(-0.612372435695796,0.707106781186546,-0.353553390593275));
#3190=DIRECTION('ref_axis',(-0.755928946018453,-0.654653670707979,0.));
#3191=DIRECTION('center_axis',(-0.612372435695796,0.707106781186546,-0.353553390593275));
#3192=DIRECTION('ref_axis',(-0.755928946018453,-0.654653670707979,0.));
#3193=DIRECTION('center_axis',(0.612372435695796,-0.707106781186546,0.353553390593275));
#3194=DIRECTION('ref_axis',(0.755928946018453,0.654653670707979,0.));
#3195=DIRECTION('',(-0.612372435695796,0.707106781186546,-0.353553390593275));
#3196=DIRECTION('center_axis',(-0.612372435695796,0.707106781186546,-0.353553390593275));
#3197=DIRECTION('ref_axis',(-0.755928946018453,-0.654653670707979,0.));
#3198=DIRECTION('center_axis',(-0.612372435695796,0.707106781186546,-0.353553390593275));
#3199=DIRECTION('ref_axis',(-0.755928946018453,-0.654653670707979,0.));
#3200=DIRECTION('',(0.101509781932626,0.962910049886276,-0.250000000000001));
#3201=DIRECTION('center_axis',(0.612372435695796,-0.707106781186546,0.353553390593275));
#3202=DIRECTION('ref_axis',(0.5,0.,-0.866025403784438));
#3203=DIRECTION('center_axis',(0.612372435695796,-0.707106781186546,0.353553390593275));
#3204=DIRECTION('ref_axis',(0.755928946018453,0.654653670707979,0.));
#3205=DIRECTION('center_axis',(-0.612372435695796,0.707106781186546,-0.353553390593275));
#3206=DIRECTION('ref_axis',(-0.755928946018453,-0.654653670707979,0.));
#3207=DIRECTION('',(0.612372435695796,-0.707106781186546,0.353553390593275));
#3208=DIRECTION('axis',(0.,0.,1.));
#3209=DIRECTION('refdir',(1.,0.,0.));
#3210=DIRECTION('center_axis',(-0.433012701892223,0.866025403784436,-0.250000000000002));
#3211=DIRECTION('ref_axis',(-0.894427190999914,-0.447213595499962,0.));
#3212=DIRECTION('center_axis',(0.433012701892223,-0.866025403784436,0.250000000000002));
#3213=DIRECTION('ref_axis',(0.894427190999914,0.447213595499962,0.));
#3214=DIRECTION('',(0.433012701892223,-0.866025403784436,0.250000000000002));
#3215=DIRECTION('center_axis',(0.433012701892223,-0.866025403784436,0.250000000000002));
#3216=DIRECTION('ref_axis',(0.894427190999914,0.447213595499962,0.));
#3217=DIRECTION('center_axis',(0.433012701892223,-0.866025403784436,0.250000000000002));
#3218=DIRECTION('ref_axis',(0.5,0.,-0.866025403784439));
#3219=DIRECTION('center_axis',(0.433012701892223,-0.866025403784437,0.250000000000002));
#3220=DIRECTION('ref_axis',(0.894427190999914,0.447213595499962,0.));
#3221=DIRECTION('center_axis',(0.433012701892223,-0.866025403784436,0.250000000000002));
#3222=DIRECTION('ref_axis',(0.5,0.,-0.866025403784439));
#3223=DIRECTION('center_axis',(-0.433012701892223,0.866025403784436,-0.250000000000002));
#3224=DIRECTION('ref_axis',(-0.894427190999914,-0.447213595499962,0.));
#3225=DIRECTION('center_axis',(-0.433012701892223,0.866025403784436,-0.250000000000002));
#3226=DIRECTION('ref_axis',(-0.894427190999914,-0.447213595499962,0.));
#3227=DIRECTION('center_axis',(0.433012701892223,-0.866025403784437,0.250000000000002));
#3228=DIRECTION('ref_axis',(0.894427190999914,0.447213595499962,0.));
#3229=DIRECTION('',(-0.433012701892223,0.866025403784436,-0.250000000000002));
#3230=DIRECTION('center_axis',(-0.433012701892223,0.866025403784436,-0.250000000000002));
#3231=DIRECTION('ref_axis',(-0.894427190999914,-0.447213595499962,0.));
#3232=DIRECTION('center_axis',(-0.433012701892223,0.866025403784436,-0.250000000000002));
#3233=DIRECTION('ref_axis',(-0.894427190999914,-0.447213595499962,0.));
#3234=DIRECTION('',(0.326269314185767,0.928600201712636,-0.17677669529664));
#3235=DIRECTION('center_axis',(0.433012701892223,-0.866025403784437,0.250000000000002));
#3236=DIRECTION('ref_axis',(0.5,0.,-0.866025403784439));
#3237=DIRECTION('center_axis',(0.433012701892223,-0.866025403784437,0.250000000000002));
#3238=DIRECTION('ref_axis',(0.894427190999914,0.447213595499962,0.));
#3239=DIRECTION('center_axis',(-0.433012701892223,0.866025403784436,-0.250000000000002));
#3240=DIRECTION('ref_axis',(-0.894427190999914,-0.447213595499962,0.));
#3241=DIRECTION('',(0.433012701892223,-0.866025403784436,0.250000000000002));
#3242=DIRECTION('axis',(0.,0.,1.));
#3243=DIRECTION('refdir',(1.,0.,0.));
#3244=DIRECTION('center_axis',(-0.224143868042018,0.965925826289067,-0.129409522551263));
#3245=DIRECTION('ref_axis',(-0.974116947696296,-0.22604462437946,0.));
#3246=DIRECTION('center_axis',(0.224143868042018,-0.965925826289067,0.129409522551263));
#3247=DIRECTION('ref_axis',(0.974116947696296,0.22604462437946,0.));
#3248=DIRECTION('',(0.224143868042018,-0.965925826289067,0.129409522551263));
#3249=DIRECTION('center_axis',(0.224143868042018,-0.965925826289067,0.129409522551263));
#3250=DIRECTION('ref_axis',(0.974116947696296,0.22604462437946,0.));
#3251=DIRECTION('center_axis',(0.224143868042018,-0.965925826289067,0.129409522551263));
#3252=DIRECTION('ref_axis',(0.,-0.132788176096111,-0.991144439670156));
#3253=DIRECTION('center_axis',(0.224143868042018,-0.965925826289067,0.129409522551263));
#3254=DIRECTION('ref_axis',(0.974116947696296,0.22604462437946,0.));
#3255=DIRECTION('center_axis',(0.224143868042018,-0.965925826289067,0.129409522551263));
#3256=DIRECTION('ref_axis',(0.,-0.132788176096111,-0.991144439670156));
#3257=DIRECTION('center_axis',(-0.224143868042018,0.965925826289067,-0.129409522551263));
#3258=DIRECTION('ref_axis',(-0.974116947696296,-0.22604462437946,0.));
#3259=DIRECTION('center_axis',(-0.224143868042018,0.965925826289067,-0.129409522551263));
#3260=DIRECTION('ref_axis',(-0.974116947696296,-0.22604462437946,0.));
#3261=DIRECTION('center_axis',(0.224143868042018,-0.965925826289067,0.129409522551263));
#3262=DIRECTION('ref_axis',(0.974116947696296,0.22604462437946,0.));
#3263=DIRECTION('',(-0.224143868042018,0.965925826289067,-0.129409522551263));
#3264=DIRECTION('center_axis',(-0.224143868042018,0.965925826289067,-0.129409522551263));
#3265=DIRECTION('ref_axis',(-0.974116947696296,-0.22604462437946,0.));
#3266=DIRECTION('center_axis',(-0.224143868042018,0.965925826289067,-0.129409522551263));
#3267=DIRECTION('ref_axis',(-0.974116947696296,-0.22604462437946,0.));
#3268=DIRECTION('',(0.530311050330904,0.842850388641698,-0.091506350946111));
#3269=DIRECTION('center_axis',(0.224143868042018,-0.965925826289067,0.129409522551263));
#3270=DIRECTION('ref_axis',(0.,-0.132788176096111,-0.991144439670156));
#3271=DIRECTION('center_axis',(0.224143868042018,-0.965925826289067,0.129409522551263));
#3272=DIRECTION('ref_axis',(0.974116947696296,0.22604462437946,0.));
#3273=DIRECTION('center_axis',(-0.224143868042018,0.965925826289067,-0.129409522551263));
#3274=DIRECTION('ref_axis',(-0.974116947696296,-0.22604462437946,0.));
#3275=DIRECTION('',(0.224143868042018,-0.965925826289067,0.129409522551263));
#3276=DIRECTION('axis',(0.,0.,1.));
#3277=DIRECTION('refdir',(1.,0.,0.));
#3278=DIRECTION('center_axis',(0.,1.,0.));
#3279=DIRECTION('ref_axis',(0.,0.,1.));
#3280=DIRECTION('center_axis',(0.,1.,0.));
#3281=DIRECTION('ref_axis',(0.,0.,1.));
#3282=DIRECTION('',(0.,-1.,0.));
#3283=DIRECTION('center_axis',(0.,1.,0.));
#3284=DIRECTION('ref_axis',(0.,0.,1.));
#3285=DIRECTION('center_axis',(0.,1.,0.));
#3286=DIRECTION('ref_axis',(0.,0.,1.));
#3287=DIRECTION('center_axis',(0.,-1.,0.));
#3288=DIRECTION('ref_axis',(0.,0.,-1.));
#3289=DIRECTION('center_axis',(0.,1.,0.));
#3290=DIRECTION('ref_axis',(0.,0.,1.));
#3291=DIRECTION('center_axis',(0.,1.,0.));
#3292=DIRECTION('ref_axis',(0.,0.,1.));
#3293=DIRECTION('center_axis',(0.,1.,0.));
#3294=DIRECTION('ref_axis',(0.,0.,1.));
#3295=DIRECTION('center_axis',(0.,1.,0.));
#3296=DIRECTION('ref_axis',(0.,0.,1.));
#3297=DIRECTION('',(0.,1.,0.));
#3298=DIRECTION('center_axis',(0.,1.,0.));
#3299=DIRECTION('ref_axis',(0.,0.,1.));
#3300=DIRECTION('center_axis',(0.,1.,0.));
#3301=DIRECTION('ref_axis',(0.,0.,1.));
#3302=DIRECTION('',(-8.65956056235494E-17,0.707106781186548,-0.707106781186548));
#3303=DIRECTION('center_axis',(0.,-1.,0.));
#3304=DIRECTION('ref_axis',(0.,0.,-1.));
#3305=DIRECTION('center_axis',(0.,-1.,0.));
#3306=DIRECTION('ref_axis',(0.,0.,-1.));
#3307=DIRECTION('center_axis',(0.,1.,0.));
#3308=DIRECTION('ref_axis',(0.,0.,1.));
#3309=DIRECTION('',(0.,-1.,0.));
#3310=DIRECTION('',(0.203483849605909,0.433012701892223,0.878119765720802));
#3311=DIRECTION('',(0.963079135454496,-0.249999999999995,-0.0998928368414017));
#3312=DIRECTION('',(-0.582080363275103,0.706518960655588,0.402508892974643));
#3313=DIRECTION('',(0.651936057602406,0.701341065416795,-0.288270856587806));
#3314=DIRECTION('',(-0.596649370647445,0.767036804266037,-0.235932340740628));
#3315=DIRECTION('',(0.789972146757459,0.509627960744633,-0.340915457224631));
#3316=DIRECTION('',(-0.763916836935503,0.491742169115809,-0.417876423550952));
#3317=DIRECTION('',(0.644741097319294,0.554304778245636,-0.52636026658703));
#3318=DIRECTION('',(0.294594207717075,0.499967294374994,-0.814399752784157));
#3319=DIRECTION('',(0.939223802390978,0.00571878967484781,0.343257839629173));
#3320=DIRECTION('',(-0.490081390490008,-0.857180169929474,0.15831104501916));
#3321=DIRECTION('',(0.17360230876733,0.0819974747248357,0.98139627701016));
#3322=DIRECTION('',(-0.0586563478610911,0.150661209273828,-0.986843773287214));
#3323=DIRECTION('',(0.601865548531004,-0.783338540141622,-0.155365996988613));
#3324=DIRECTION('',(-0.836357327772553,-0.374481435442469,0.400337451146034));
#3325=DIRECTION('',(0.318384369676236,0.262663105372072,0.9108454787845));
#3326=DIRECTION('',(-0.367977985664953,-0.392555368823596,-0.842907162428778));
#3327=DIRECTION('',(0.629580921974141,-0.772291066116685,0.0848196432587745));
#3328=DIRECTION('',(-0.97842647478805,-0.140452579010683,0.151508106987968));
#3329=DIRECTION('',(0.0948179722037916,0.346271397002718,0.933330419393339));
#3330=DIRECTION('',(-0.678151608737242,-0.35128959010514,-0.64552770618375));
#3331=DIRECTION('',(0.433295742654717,-0.900576175248329,0.0348905713966902));
#3332=DIRECTION('',(-0.316000619316692,0.499967294375032,0.806335112187716));
#3333=DIRECTION('',(0.932239618762088,0.00571878967484657,0.361796335878312));
#3334=DIRECTION('',(-0.0107032057998375,-0.999934588749994,-0.00403232029813605));
#3335=DIRECTION('',(0.935731710576533,-0.011437579349689,0.352527087753742));
#3336=CARTESIAN_POINT('',(0.,0.,0.));
#3337=CARTESIAN_POINT('',(0.,0.,0.));
#3338=CARTESIAN_POINT('Origin',(-69.7150450046476,109.,-52.2499999999992));
#3339=CARTESIAN_POINT('',(-57.0362860918569,101.937180526611,-60.2102546138697));
#3340=CARTESIAN_POINT('',(-60.5003877069947,101.937180526611,-62.2102546138697));
#3341=CARTESIAN_POINT('',(-60.5003877069947,101.937180526611,-62.2102546138697));
#3342=CARTESIAN_POINT('',(-63.4028671781572,123.991664350565,-49.1830127018903));
#3343=CARTESIAN_POINT('Origin',(-63.6528671781565,109.,-48.7499999999993));
#3344=CARTESIAN_POINT('',(-66.866968793295,123.991664350565,-51.1830127018903));
#3345=CARTESIAN_POINT('',(-66.866968793295,123.991664350565,-51.1830127018903));
#3346=CARTESIAN_POINT('Origin',(-67.1169687932943,109.,-50.7499999999993));
#3347=CARTESIAN_POINT('Origin',(-69.7150450046476,109.,-52.2499999999992));
#3348=CARTESIAN_POINT('',(-60.7503877069946,101.071155122826,-61.7772419119775));
#3349=CARTESIAN_POINT('',(-57.2862860918569,101.071155122826,-59.7772419119775));
#3350=CARTESIAN_POINT('',(-60.7503877069946,101.071155122826,-61.7772419119775));
#3351=CARTESIAN_POINT('',(-73.4835498795932,101.071155122824,-39.7227580880222));
#3352=CARTESIAN_POINT('Origin',(-67.1169687932943,109.,-50.7499999999993));
#3353=CARTESIAN_POINT('',(-70.0194482644555,101.071155122824,-37.7227580880222));
#3354=CARTESIAN_POINT('',(-73.4835498795932,101.071155122824,-39.7227580880221));
#3355=CARTESIAN_POINT('Origin',(-63.6528671781565,109.,-48.7499999999993));
#3356=CARTESIAN_POINT('Origin',(-119.078493020361,109.,-80.7499999999988));
#3357=CARTESIAN_POINT('',(-65.5747753124034,96.49269543419,-59.421157464004));
#3358=CARTESIAN_POINT('',(-73.855314696892,96.4926954341901,-45.0788425359943));
#3359=CARTESIAN_POINT('Origin',(-69.7150450046476,109.,-52.2499999999992));
#3360=CARTESIAN_POINT('',(-123.218762712605,96.4926954341901,-73.5788425359939));
#3361=CARTESIAN_POINT('',(-123.218762712605,96.4926954341901,-73.5788425359939));
#3362=CARTESIAN_POINT('',(-114.938223328117,96.49269543419,-87.9211574640035));
#3363=CARTESIAN_POINT('Origin',(-119.078493020361,109.,-80.7499999999988));
#3364=CARTESIAN_POINT('',(-114.938223328117,96.49269543419,-87.9211574640035));
#3365=CARTESIAN_POINT('Origin',(-119.078493020361,109.,-80.7499999999988));
#3366=CARTESIAN_POINT('',(-94.3860089394201,105.235685467736,-49.7275542973482));
#3367=CARTESIAN_POINT('',(-82.8207084929668,105.235685467736,-43.0503249713298));
#3368=CARTESIAN_POINT('',(-94.3860089394201,105.235685467737,-49.7275542973482));
#3369=CARTESIAN_POINT('',(-91.0176401746589,103.250749366077,-48.5513043322017));
#3370=CARTESIAN_POINT('Ctrl Pts',(-91.0176401746589,103.250749366077,-48.5513043322017));
#3371=CARTESIAN_POINT('Ctrl Pts',(-91.2361059276669,103.557750420993,-48.5303294493383));
#3372=CARTESIAN_POINT('Ctrl Pts',(-91.4832335600058,103.842139746856,-48.5508334265686));
#3373=CARTESIAN_POINT('Ctrl Pts',(-92.1066673879442,104.430592760333,-48.6750977465524));
#3374=CARTESIAN_POINT('Ctrl Pts',(-92.5431699718694,104.735168552794,-48.8223964645982));
#3375=CARTESIAN_POINT('Ctrl Pts',(-93.461912716518,105.137985045737,-49.2219363914119));
#3376=CARTESIAN_POINT('Ctrl Pts',(-93.9449426785634,105.235685467736,-49.4729045729122));
#3377=CARTESIAN_POINT('Ctrl Pts',(-94.3860089394201,105.235685467736,-49.7275542973483));
#3378=CARTESIAN_POINT('',(-92.3860089394197,98.3074822374609,-53.1916559124865));
#3379=CARTESIAN_POINT('Ctrl Pts',(-92.3860089394197,98.307482237461,-53.1916559124864));
#3380=CARTESIAN_POINT('Ctrl Pts',(-91.944942678563,98.307482237461,-52.9370061880504));
#3381=CARTESIAN_POINT('Ctrl Pts',(-91.5102607802988,98.3772644212952,-52.6022967036335));
#3382=CARTESIAN_POINT('Ctrl Pts',(-90.7942826050959,98.676845000861,-51.8515582405649));
#3383=CARTESIAN_POINT('Ctrl Pts',(-90.5123369230427,98.9076700218055,-51.4365591158164));
#3384=CARTESIAN_POINT('Ctrl Pts',(-90.1413389560881,99.4578375470661,-50.6726253387866));
#3385=CARTESIAN_POINT('Ctrl Pts',(-90.0255053791506,99.8112989429842,-50.2740223286365));
#3386=CARTESIAN_POINT('Ctrl Pts',(-89.9729277960154,100.614428273412,-49.573341944019));
#3387=CARTESIAN_POINT('Ctrl Pts',(-90.0353007740436,101.064744995698,-49.2720751413297));
#3388=CARTESIAN_POINT('Ctrl Pts',(-90.2865953679429,101.9352550043,-48.8368201370289));
#3389=CARTESIAN_POINT('Ctrl Pts',(-90.4922380489042,102.413371759201,-48.6738702011243));
#3390=CARTESIAN_POINT('Ctrl Pts',(-90.8440070426079,102.99654996933,-48.5751774684912));
#3391=CARTESIAN_POINT('Ctrl Pts',(-90.9285040512729,103.125489990024,-48.559862285662));
#3392=CARTESIAN_POINT('Ctrl Pts',(-91.0176401746589,103.250749366077,-48.5513043322017));
#3393=CARTESIAN_POINT('',(-80.8207084929665,98.3074822374608,-46.5144265864682));
#3394=CARTESIAN_POINT('',(-92.3860089394198,98.3074822374611,-53.1916559124864));
#3395=CARTESIAN_POINT('',(-84.4784050214276,104.702740240336,-44.1791103605043));
#3396=CARTESIAN_POINT('Ctrl Pts',(-84.4784050214273,104.702740240336,-44.179110360504));
#3397=CARTESIAN_POINT('Ctrl Pts',(-84.719910157753,104.526945752297,-44.3792409314819));
#3398=CARTESIAN_POINT('Ctrl Pts',(-84.9292227283709,104.313493521274,-44.5780840276366));
#3399=CARTESIAN_POINT('Ctrl Pts',(-85.3433081511931,103.743726568118,-45.0453786543482));
#3400=CARTESIAN_POINT('Ctrl Pts',(-85.5286602574863,103.319666529342,-45.3392616445606));
#3401=CARTESIAN_POINT('Ctrl Pts',(-85.6804888744289,102.416155145618,-45.8942563092267));
#3402=CARTESIAN_POINT('Ctrl Pts',(-85.6462202716666,101.937209973523,-46.1563950132377));
#3403=CARTESIAN_POINT('Ctrl Pts',(-85.3937969757602,101.062790026475,-46.5936049867616));
#3404=CARTESIAN_POINT('Ctrl Pts',(-85.1596379659028,100.611874672147,-46.7963965459624));
#3405=CARTESIAN_POINT('Ctrl Pts',(-84.5153961509797,99.8096167014324,-47.0942865585158));
#3406=CARTESIAN_POINT('Ctrl Pts',(-84.1059621410022,99.4574342557325,-47.1885248105415));
#3407=CARTESIAN_POINT('Ctrl Pts',(-83.2575101221815,98.9126166677475,-47.2430172368065));
#3408=CARTESIAN_POINT('Ctrl Pts',(-82.7609372275344,98.6829050367047,-47.2068324926174));
#3409=CARTESIAN_POINT('Ctrl Pts',(-81.7609021788356,98.3807025943171,-46.9694819795316));
#3410=CARTESIAN_POINT('Ctrl Pts',(-81.2579982865691,98.3074822374608,-46.7668959665184));
#3411=CARTESIAN_POINT('Ctrl Pts',(-80.8207084929665,98.3074822374608,-46.5144265864681));
#3412=CARTESIAN_POINT('Ctrl Pts',(-82.8207084929668,105.235685467736,-43.0503249713298));
#3413=CARTESIAN_POINT('Ctrl Pts',(-83.2579982865694,105.235685467736,-43.3027943513801));
#3414=CARTESIAN_POINT('Ctrl Pts',(-83.7101950061769,105.133251025885,-43.5932077637468));
#3415=CARTESIAN_POINT('Ctrl Pts',(-84.2375848518395,104.864030249166,-43.985328869011));
#3416=CARTESIAN_POINT('Ctrl Pts',(-84.3616836412502,104.787703134226,-44.0823856414543));
#3417=CARTESIAN_POINT('Ctrl Pts',(-84.4784050214273,104.702740240336,-44.179110360504));
#3418=CARTESIAN_POINT('Origin',(-119.078493020361,109.,-80.7499999999988));
#3419=CARTESIAN_POINT('',(-105.931810542547,105.235685467737,-56.3935259609235));
#3420=CARTESIAN_POINT('',(-105.931810542547,105.235685467737,-56.3935259609236));
#3421=CARTESIAN_POINT('',(-102.208219994794,103.102717662028,-55.0841964154936));
#3422=CARTESIAN_POINT('Ctrl Pts',(-102.208219994794,103.102717662026,-55.0841964154936));
#3423=CARTESIAN_POINT('Ctrl Pts',(-102.449021592923,103.452288080539,-55.0506293513879));
#3424=CARTESIAN_POINT('Ctrl Pts',(-102.730142130046,103.775612080798,-55.0719387240821));
#3425=CARTESIAN_POINT('Ctrl Pts',(-103.427690853637,104.41668799164,-55.2155771708353));
#3426=CARTESIAN_POINT('Ctrl Pts',(-103.909507673844,104.73291730259,-55.385468864601));
#3427=CARTESIAN_POINT('Ctrl Pts',(-104.920531073176,105.142197830513,-55.8362211929756));
#3428=CARTESIAN_POINT('Ctrl Pts',(-105.450263434612,105.235685467736,-56.1155046085297));
#3429=CARTESIAN_POINT('Ctrl Pts',(-105.931810542547,105.235685467736,-56.3935259609236));
#3430=CARTESIAN_POINT('',(-103.931810542547,98.307482237461,-59.8576275760617));
#3431=CARTESIAN_POINT('Ctrl Pts',(-103.931810542547,98.3074822374611,-59.8576275760617));
#3432=CARTESIAN_POINT('Ctrl Pts',(-103.450263434612,98.3074822374611,-59.5796062236677));
#3433=CARTESIAN_POINT('Ctrl Pts',(-102.966762319561,98.3741443355121,-59.2202479404765));
#3434=CARTESIAN_POINT('Ctrl Pts',(-102.161749770577,98.6785063270139,-58.4126743523891));
#3435=CARTESIAN_POINT('Ctrl Pts',(-101.840308730574,98.9178350152992,-57.9650036590062));
#3436=CARTESIAN_POINT('Ctrl Pts',(-101.440098436538,99.4841271059821,-57.1713087801904));
#3437=CARTESIAN_POINT('Ctrl Pts',(-101.317391802105,99.8312991080725,-56.7758910574572));
#3438=CARTESIAN_POINT('Ctrl Pts',(-101.255012945074,100.623349028226,-56.0804534046886));
#3439=CARTESIAN_POINT('Ctrl Pts',(-101.314116564966,101.068801289505,-55.7811982784879));
#3440=CARTESIAN_POINT('Ctrl Pts',(-101.563069256545,101.931198710494,-55.3499995679935));
#3441=CARTESIAN_POINT('Ctrl Pts',(-101.769030711735,102.403958803925,-55.1901485168392));
#3442=CARTESIAN_POINT('Ctrl Pts',(-102.095779742704,102.93486881927,-55.1031827978842));
#3443=CARTESIAN_POINT('Ctrl Pts',(-102.150902897407,103.019510732018,-55.0921862573272));
#3444=CARTESIAN_POINT('Ctrl Pts',(-102.208219994794,103.102717662026,-55.0841964154936));
#3445=CARTESIAN_POINT('',(-103.931810542547,98.3074822374611,-59.8576275760617));
#3446=CARTESIAN_POINT('Ctrl Pts',(-94.3860089394201,105.235685467736,-49.7275542973483));
#3447=CARTESIAN_POINT('Ctrl Pts',(-94.8437110509037,105.235685467736,-49.991808734622));
#3448=CARTESIAN_POINT('Ctrl Pts',(-95.3183294965658,105.131719766023,-50.2956435885911));
#3449=CARTESIAN_POINT('Ctrl Pts',(-96.1649446403336,104.726122671488,-50.9165050382747));
#3450=CARTESIAN_POINT('Ctrl Pts',(-96.5365223340826,104.425439262705,-51.2347212917227));
#3451=CARTESIAN_POINT('Ctrl Pts',(-97.079067270285,103.751330105903,-51.8179767152385));
#3452=CARTESIAN_POINT('Ctrl Pts',(-97.2914477713889,103.33295780308,-52.124268380383));
#3453=CARTESIAN_POINT('Ctrl Pts',(-97.4838471817179,102.430163538116,-52.7010684635898));
#3454=CARTESIAN_POINT('Ctrl Pts',(-97.4623083504636,101.946025606973,-52.9725395573328));
#3455=CARTESIAN_POINT('Ctrl Pts',(-97.2047953462119,101.053974393026,-53.4185651643064));
#3456=CARTESIAN_POINT('Ctrl Pts',(-96.9552287340129,100.59897551963,-53.616662472833));
#3457=CARTESIAN_POINT('Ctrl Pts',(-96.2710769848093,99.7982897132515,-53.8916024252977));
#3458=CARTESIAN_POINT('Ctrl Pts',(-95.8377694343555,99.451348267594,-53.9679676343933));
#3459=CARTESIAN_POINT('Ctrl Pts',(-94.9448662844064,98.9117809702792,-53.991550437936));
#3460=CARTESIAN_POINT('Ctrl Pts',(-94.4206402272791,98.683674936935,-53.9377289055515));
#3461=CARTESIAN_POINT('Ctrl Pts',(-93.3698028357836,98.3818254132703,-53.670590764968));
#3462=CARTESIAN_POINT('Ctrl Pts',(-92.8437110509033,98.307482237461,-53.4559103497602));
#3463=CARTESIAN_POINT('Ctrl Pts',(-92.3860089394197,98.307482237461,-53.1916559124864));
#3464=CARTESIAN_POINT('Origin',(-119.078493020361,109.,-80.7499999999988));
#3465=CARTESIAN_POINT('',(-117.424340315019,105.235685467737,-63.0287411187298));
#3466=CARTESIAN_POINT('',(-117.424340315019,105.235685467737,-63.0287411187298));
#3467=CARTESIAN_POINT('',(-112.873099678569,102.847499823892,-61.3708278876974));
#3468=CARTESIAN_POINT('Ctrl Pts',(-112.873099678569,102.847499823892,-61.3708278876974));
#3469=CARTESIAN_POINT('Ctrl Pts',(-112.885263071986,102.865530125643,-61.3684870415431));
#3470=CARTESIAN_POINT('Ctrl Pts',(-112.897548248638,102.883504310233,-61.366295141775));
#3471=CARTESIAN_POINT('Ctrl Pts',(-113.223445655223,103.354153784421,-61.312605698808));
#3472=CARTESIAN_POINT('Ctrl Pts',(-113.617943081627,103.765699546249,-61.3609453836262));
#3473=CARTESIAN_POINT('Ctrl Pts',(-114.51341914509,104.46875863804,-61.596335766007));
#3474=CARTESIAN_POINT('Ctrl Pts',(-115.084650741731,104.772419738951,-61.8242044014969));
#3475=CARTESIAN_POINT('Ctrl Pts',(-116.26458534071,105.155153282331,-62.3819677418281));
#3476=CARTESIAN_POINT('Ctrl Pts',(-116.873387883958,105.235685467737,-62.7106485843461));
#3477=CARTESIAN_POINT('Ctrl Pts',(-117.424340315019,105.235685467736,-63.0287411187299));
#3478=CARTESIAN_POINT('',(-115.424340315019,98.3074822374612,-66.4928427338677));
#3479=CARTESIAN_POINT('Ctrl Pts',(-115.424340315019,98.3074822374612,-66.4928427338678));
#3480=CARTESIAN_POINT('Ctrl Pts',(-114.873387883957,98.3074822374612,-66.1747501994839));
#3481=CARTESIAN_POINT('Ctrl Pts',(-114.304395627967,98.3648569324462,-65.7771159167707));
#3482=CARTESIAN_POINT('Ctrl Pts',(-113.316922034078,98.6488278676478,-64.8860003371488));
#3483=CARTESIAN_POINT('Ctrl Pts',(-112.899248494017,98.8771074785532,-64.3921613457507));
#3484=CARTESIAN_POINT('Ctrl Pts',(-112.369176942676,99.4398467473837,-63.5238717830588));
#3485=CARTESIAN_POINT('Ctrl Pts',(-112.191730388089,99.7801872611806,-63.0995889604281));
#3486=CARTESIAN_POINT('Ctrl Pts',(-112.057561335007,100.581884791004,-62.3492963885222));
#3487=CARTESIAN_POINT('Ctrl Pts',(-112.099359165682,101.044133890221,-62.0245059301422));
#3488=CARTESIAN_POINT('Ctrl Pts',(-112.357346552702,101.937828414283,-61.5776586681113));
#3489=CARTESIAN_POINT('Ctrl Pts',(-112.577858013516,102.409850877713,-61.4276471726289));
#3490=CARTESIAN_POINT('Ctrl Pts',(-112.873099678569,102.847499823891,-61.3708278876975));
#3491=CARTESIAN_POINT('',(-115.424340315019,98.3074822374611,-66.4928427338679));
#3492=CARTESIAN_POINT('Ctrl Pts',(-105.931810542547,105.235685467736,-56.3935259609236));
#3493=CARTESIAN_POINT('Ctrl Pts',(-106.441097653729,105.235685467736,-56.687563011659));
#3494=CARTESIAN_POINT('Ctrl Pts',(-106.974640486628,105.132960205187,-57.0250658019486));
#3495=CARTESIAN_POINT('Ctrl Pts',(-107.947581410815,104.730808636537,-57.7176366639949));
#3496=CARTESIAN_POINT('Ctrl Pts',(-108.386686426508,104.432320373104,-58.0736604657704));
#3497=CARTESIAN_POINT('Ctrl Pts',(-109.030432576161,103.765790736202,-58.7123084319066));
#3498=CARTESIAN_POINT('Ctrl Pts',(-109.294438065739,103.359086193815,-59.0420063444297));
#3499=CARTESIAN_POINT('Ctrl Pts',(-109.56709842014,102.458977333711,-59.6612621436709));
#3500=CARTESIAN_POINT('Ctrl Pts',(-109.572926265459,101.965344390994,-59.9517288812603));
#3501=CARTESIAN_POINT('Ctrl Pts',(-109.304259556052,101.034655609004,-60.4170732722551));
#3502=CARTESIAN_POINT('Ctrl Pts',(-109.022522963702,100.572512615502,-60.6044945027757));
#3503=CARTESIAN_POINT('Ctrl Pts',(-108.260113770694,99.7760817327768,-60.8335085749491));
#3504=CARTESIAN_POINT('Ctrl Pts',(-107.781619042588,99.4397737575475,-60.8753169212342));
#3505=CARTESIAN_POINT('Ctrl Pts',(-106.791454021988,98.9062732240887,-60.8366840402783));
#3506=CARTESIAN_POINT('Ctrl Pts',(-106.200906509653,98.6801492903,-60.7429663371135));
#3507=CARTESIAN_POINT('Ctrl Pts',(-105.025500473564,98.3809411378044,-60.40107533564));
#3508=CARTESIAN_POINT('Ctrl Pts',(-104.441097653728,98.3074822374611,-60.1516646267969));
#3509=CARTESIAN_POINT('Ctrl Pts',(-103.931810542547,98.3074822374611,-59.8576275760616));
#3510=CARTESIAN_POINT('Origin',(-119.078493020361,109.,-80.7499999999988));
#3511=CARTESIAN_POINT('',(-118.78998649473,98.3074822374612,-68.4359994617213));
#3512=CARTESIAN_POINT('',(-118.78998649473,98.3074822374611,-68.4359994617214));
#3513=CARTESIAN_POINT('Ctrl Pts',(-117.424340315019,105.235685467736,-63.0287411187299));
#3514=CARTESIAN_POINT('Ctrl Pts',(-118.104455067791,105.235685467737,-63.4214055543222));
#3515=CARTESIAN_POINT('Ctrl Pts',(-118.823383370921,105.115025708115,-63.8707727019096));
#3516=CARTESIAN_POINT('Ctrl Pts',(-120.152211057545,104.638615075121,-64.7952439254207));
#3517=CARTESIAN_POINT('Ctrl Pts',(-120.762708154872,104.285378551405,-65.27078272247));
#3518=CARTESIAN_POINT('Ctrl Pts',(-121.530321038309,103.561110088859,-66.0199577490771));
#3519=CARTESIAN_POINT('Ctrl Pts',(-121.807474740758,103.201357059968,-66.343360523086));
#3520=CARTESIAN_POINT('Ctrl Pts',(-122.043414724861,102.594072465734,-66.7981024939494));
#3521=CARTESIAN_POINT('Ctrl Pts',(-122.092678493038,102.380375656682,-66.945003657385));
#3522=CARTESIAN_POINT('Ctrl Pts',(-122.117297884372,101.943528113597,-67.2175789887018));
#3523=CARTESIAN_POINT('Ctrl Pts',(-122.092529257229,101.720365047742,-67.3432446008741));
#3524=CARTESIAN_POINT('Ctrl Pts',(-121.965301437595,101.279634952257,-67.5636096486164));
#3525=CARTESIAN_POINT('Ctrl Pts',(-121.863134141106,101.063079080039,-67.6578035054809));
#3526=CARTESIAN_POINT('Ctrl Pts',(-121.5934173484,100.650884319169,-67.8097493261416));
#3527=CARTESIAN_POINT('Ctrl Pts',(-121.425973083727,100.45519187943,-67.8675427871017));
#3528=CARTESIAN_POINT('Ctrl Pts',(-120.858109129937,99.9126581141667,-67.9877099959866));
#3529=CARTESIAN_POINT('Ctrl Pts',(-120.389803254753,99.6102405927516,-67.9953924971306));
#3530=CARTESIAN_POINT('Ctrl Pts',(-119.242323386653,99.0186112201875,-67.9041663880787));
#3531=CARTESIAN_POINT('Ctrl Pts',(-118.452225355267,98.7496918581534,-67.7397055339048));
#3532=CARTESIAN_POINT('Ctrl Pts',(-116.883055382911,98.393532390957,-67.231519360489));
#3533=CARTESIAN_POINT('Ctrl Pts',(-116.10445506779,98.3074822374612,-66.8855071694601));
#3534=CARTESIAN_POINT('Ctrl Pts',(-115.424340315019,98.3074822374612,-66.4928427338678));
#3535=CARTESIAN_POINT('',(-120.78998649473,105.235685467737,-64.9718978465832));
#3536=CARTESIAN_POINT('',(-120.78998649473,105.235685467737,-64.9718978465831));
#3537=CARTESIAN_POINT('Ctrl Pts',(-118.78998649473,98.3074822374612,-68.4359994617213));
#3538=CARTESIAN_POINT('Ctrl Pts',(-118.918348276834,98.3074822374612,-68.5101091711724));
#3539=CARTESIAN_POINT('Ctrl Pts',(-119.051966028522,98.319606062948,-68.5729797213706));
#3540=CARTESIAN_POINT('Ctrl Pts',(-119.390180292013,98.3776312711511,-68.7006060360938));
#3541=CARTESIAN_POINT('Ctrl Pts',(-119.594844068455,98.4360499331429,-68.7509667466566));
#3542=CARTESIAN_POINT('Ctrl Pts',(-120.108561068232,98.6351217911646,-68.822841039124));
#3543=CARTESIAN_POINT('Ctrl Pts',(-120.410333239601,98.8023575570841,-68.8132768624661));
#3544=CARTESIAN_POINT('Ctrl Pts',(-121.095658711484,99.2862798538955,-68.7087637376292));
#3545=CARTESIAN_POINT('Ctrl Pts',(-121.453647702316,99.6436546824008,-68.5719722406892));
#3546=CARTESIAN_POINT('Ctrl Pts',(-121.95322023847,100.313709548206,-68.2828712619504));
#3547=CARTESIAN_POINT('Ctrl Pts',(-122.13026373805,100.619480486203,-68.1403943115824));
#3548=CARTESIAN_POINT('Ctrl Pts',(-122.350414930589,101.118875846441,-67.8997101912188));
#3549=CARTESIAN_POINT('Ctrl Pts',(-122.419254299142,101.308117977183,-67.8067240343058));
#3550=CARTESIAN_POINT('Ctrl Pts',(-122.529732701345,101.690626616667,-67.6154765320548));
#3551=CARTESIAN_POINT('Ctrl Pts',(-122.571615353665,101.884694244957,-67.5168156573903));
#3552=CARTESIAN_POINT('Ctrl Pts',(-122.647401154913,102.409372784178,-67.2455011686517));
#3553=CARTESIAN_POINT('Ctrl Pts',(-122.655932486104,102.745023337843,-67.0673187398412));
#3554=CARTESIAN_POINT('Ctrl Pts',(-122.572273917842,103.513663673561,-66.6372167411127));
#3555=CARTESIAN_POINT('Ctrl Pts',(-122.443353045988,103.95119638048,-66.3765548091624));
#3556=CARTESIAN_POINT('Ctrl Pts',(-122.075417244245,104.56927639081,-65.9299074078767));
#3557=CARTESIAN_POINT('Ctrl Pts',(-121.885875205944,104.790787749988,-65.7451136026938));
#3558=CARTESIAN_POINT('Ctrl Pts',(-121.506987477856,105.058995953627,-65.4396037944961));
#3559=CARTESIAN_POINT('Ctrl Pts',(-121.342237738227,105.139116769073,-65.3199491226463));
#3560=CARTESIAN_POINT('Ctrl Pts',(-121.043690674034,105.218909586375,-65.1233635722866));
#3561=CARTESIAN_POINT('Ctrl Pts',(-120.918381560469,105.235685467737,-65.0460267723497));
#3562=CARTESIAN_POINT('Ctrl Pts',(-120.78998649473,105.235685467737,-64.9718978465831));
#3563=CARTESIAN_POINT('Origin',(-119.078493020361,109.,-80.7499999999988));
#3564=CARTESIAN_POINT('',(-66.3693581073396,122.42480974691,-58.0448996923544));
#3565=CARTESIAN_POINT('',(-62.2290884150953,108.0824948189,-65.2160571563592));
#3566=CARTESIAN_POINT('Origin',(-69.7150450046476,109.,-52.2499999999992));
#3567=CARTESIAN_POINT('',(-111.592536430809,108.0824948189,-93.7160571563587));
#3568=CARTESIAN_POINT('',(-111.592536430809,108.0824948189,-93.7160571563587));
#3569=CARTESIAN_POINT('',(-115.732806123053,122.42480974691,-86.5448996923539));
#3570=CARTESIAN_POINT('Origin',(-119.078493020361,109.,-80.7499999999988));
#3571=CARTESIAN_POINT('',(-115.732806123053,122.42480974691,-86.5448996923539));
#3572=CARTESIAN_POINT('Origin',(-119.078493020361,109.,-80.7499999999988));
#3573=CARTESIAN_POINT('',(-81.8660249138711,98.3074822374625,-71.4128027395503));
#3574=CARTESIAN_POINT('',(-70.3007244674178,98.3074822374627,-64.7355734135318));
#3575=CARTESIAN_POINT('',(-81.8660249138712,98.3074822374623,-71.4128027395501));
#3576=CARTESIAN_POINT('',(-78.1372951281693,99.8763092742309,-70.8607163717404));
#3577=CARTESIAN_POINT('Ctrl Pts',(-78.1372951281693,99.8763092742309,-70.8607163717404));
#3578=CARTESIAN_POINT('Ctrl Pts',(-78.3931479940217,99.6124791386442,-70.7749851098822));
#3579=CARTESIAN_POINT('Ctrl Pts',(-78.6840646784847,99.3786530548441,-70.7196442240182));
#3580=CARTESIAN_POINT('Ctrl Pts',(-79.4092304936657,98.9076700218071,-70.6677035733428));
#3581=CARTESIAN_POINT('Ctrl Pts',(-79.9096031192728,98.6768450008626,-70.704376134114));
#3582=CARTESIAN_POINT('Ctrl Pts',(-80.9177507874897,98.3772644212968,-70.9490621908606));
#3583=CARTESIAN_POINT('Ctrl Pts',(-81.4249586530144,98.3074822374626,-71.1581530151143));
#3584=CARTESIAN_POINT('Ctrl Pts',(-81.8660249138711,98.3074822374626,-71.4128027395504));
#3585=CARTESIAN_POINT('',(-79.8660249138713,105.235685467738,-74.8769043546876));
#3586=CARTESIAN_POINT('Ctrl Pts',(-79.8660249138713,105.235685467738,-74.8769043546876));
#3587=CARTESIAN_POINT('Ctrl Pts',(-79.4249586530146,105.235685467738,-74.6222546302515));
#3588=CARTESIAN_POINT('Ctrl Pts',(-78.966098851271,105.13798504574,-74.3294225030814));
#3589=CARTESIAN_POINT('Ctrl Pts',(-78.1607157524998,104.735168552796,-73.7335379100799));
#3590=CARTESIAN_POINT('Ctrl Pts',(-77.8149000287647,104.430592760335,-73.4291649426061));
#3591=CARTESIAN_POINT('Ctrl Pts',(-77.3250662827369,103.743205497,-72.8710607726881));
#3592=CARTESIAN_POINT('Ctrl Pts',(-77.1468233216009,103.317679951548,-72.580553986839));
#3593=CARTESIAN_POINT('Ctrl Pts',(-77.0066222737195,102.413371759203,-72.0316418950969));
#3594=CARTESIAN_POINT('Ctrl Pts',(-77.0449197172773,101.935255004302,-71.7720751413298));
#3595=CARTESIAN_POINT('Ctrl Pts',(-77.2962143111765,101.0647449957,-71.3368201370292));
#3596=CARTESIAN_POINT('Ctrl Pts',(-77.5259325266081,100.614428273414,-71.1321701522025));
#3597=CARTESIAN_POINT('Ctrl Pts',(-77.9342089099037,100.096499176469,-70.9356037497933));
#3598=CARTESIAN_POINT('Ctrl Pts',(-78.0329047040169,99.9839545009761,-70.895695549162));
#3599=CARTESIAN_POINT('Ctrl Pts',(-78.1372951281693,99.8763092742309,-70.8607163717404));
#3600=CARTESIAN_POINT('',(-68.3007244674181,105.235685467739,-68.1996750286692));
#3601=CARTESIAN_POINT('',(-79.8660249138713,105.235685467738,-74.8769043546876));
#3602=CARTESIAN_POINT('',(-71.8391803616632,98.7027402403375,-66.0708896394943));
#3603=CARTESIAN_POINT('Ctrl Pts',(-71.8391803616628,98.7027402403373,-66.070889639494));
#3604=CARTESIAN_POINT('Ctrl Pts',(-72.0439884445282,98.8361606209892,-66.3345813715533));
#3605=CARTESIAN_POINT('Ctrl Pts',(-72.2115336533623,99.001384056873,-66.6057676604154));
#3606=CARTESIAN_POINT('Ctrl Pts',(-72.5271374781293,99.4574342557344,-67.2436374185692));
#3607=CARTESIAN_POINT('Ctrl Pts',(-72.6502417628557,99.8096167014344,-67.645336798396));
#3608=CARTESIAN_POINT('Ctrl Pts',(-72.7143823519123,100.611874672149,-68.3522115825761));
#3609=CARTESIAN_POINT('Ctrl Pts',(-72.6558392149002,101.062790026477,-68.6563950132379));
#3610=CARTESIAN_POINT('Ctrl Pts',(-72.4034159189938,101.937209973525,-69.0936049867617));
#3611=CARTESIAN_POINT('Ctrl Pts',(-72.1935314433864,102.41615514562,-69.2543518193115));
#3612=CARTESIAN_POINT('Ctrl Pts',(-71.6369776563495,103.319666529344,-69.4003617123507));
#3613=CARTESIAN_POINT('Ctrl Pts',(-71.2897914679388,103.743726568121,-69.3867835747619));
#3614=CARTESIAN_POINT('Ctrl Pts',(-70.5589898894586,104.424395182907,-69.2374994608244));
#3615=CARTESIAN_POINT('Ctrl Pts',(-70.1256610955174,104.727134811084,-69.0917727209338));
#3616=CARTESIAN_POINT('Ctrl Pts',(-69.2156180135337,105.133251025888,-68.6985515492242));
#3617=CARTESIAN_POINT('Ctrl Pts',(-68.7380142610207,105.235685467739,-68.4521444087194));
#3618=CARTESIAN_POINT('Ctrl Pts',(-68.3007244674181,105.235685467739,-68.1996750286692));
#3619=CARTESIAN_POINT('Ctrl Pts',(-70.3007244674178,98.3074822374626,-64.7355734135318));
#3620=CARTESIAN_POINT('Ctrl Pts',(-70.7380142610204,98.3074822374626,-64.9880427935821));
#3621=CARTESIAN_POINT('Ctrl Pts',(-71.1649108408744,98.3807025943189,-65.3222773334404));
#3622=CARTESIAN_POINT('Ctrl Pts',(-71.63264360737,98.5810373096057,-65.817727530853));
#3623=CARTESIAN_POINT('Ctrl Pts',(-71.7401949633927,98.6382570943041,-65.9434452986592));
#3624=CARTESIAN_POINT('Ctrl Pts',(-71.8391803616628,98.7027402403373,-66.070889639494));
#3625=CARTESIAN_POINT('Origin',(-119.078493020361,109.,-80.7499999999988));
#3626=CARTESIAN_POINT('',(-93.4118265169985,98.3074822374623,-78.0787744031255));
#3627=CARTESIAN_POINT('',(-93.4118265169985,98.3074822374623,-78.0787744031255));
#3628=CARTESIAN_POINT('',(-89.310545785853,100.004330985067,-77.4236234448516));
#3629=CARTESIAN_POINT('Ctrl Pts',(-89.3105457858516,100.004330985068,-77.4236234448524));
#3630=CARTESIAN_POINT('Ctrl Pts',(-89.5906127684196,99.7001003271067,-77.3220467399197));
#3631=CARTESIAN_POINT('Ctrl Pts',(-89.9201573466291,99.432691593161,-77.2594832131444));
#3632=CARTESIAN_POINT('Ctrl Pts',(-90.7270152190322,98.9178350153006,-77.2137926604239));
#3633=CARTESIAN_POINT('Ctrl Pts',(-91.275429932033,98.6785063270153,-77.2683334201939));
#3634=CARTESIAN_POINT('Ctrl Pts',(-92.3773154492341,98.3741443355135,-77.5617079439358));
#3635=CARTESIAN_POINT('Ctrl Pts',(-92.930279409063,98.3074822374625,-77.8007530507317));
#3636=CARTESIAN_POINT('Ctrl Pts',(-93.4118265169985,98.3074822374625,-78.0787744031257));
#3637=CARTESIAN_POINT('',(-91.4118265169984,105.235685467738,-81.5428760182629));
#3638=CARTESIAN_POINT('Ctrl Pts',(-91.4118265169984,105.235685467738,-81.5428760182628));
#3639=CARTESIAN_POINT('Ctrl Pts',(-90.930279409063,105.235685467738,-81.2648546658689));
#3640=CARTESIAN_POINT('Ctrl Pts',(-90.4235466956197,105.142197830515,-80.9457346914359));
#3641=CARTESIAN_POINT('Ctrl Pts',(-89.5276720287663,104.732917302591,-80.2955389079813));
#3642=CARTESIAN_POINT('Ctrl Pts',(-89.1396330959697,104.416687991642,-79.9632191485941));
#3643=CARTESIAN_POINT('Ctrl Pts',(-88.6191933845126,103.711566927935,-79.3777677293152));
#3644=CARTESIAN_POINT('Ctrl Pts',(-88.4360002798934,103.294551166156,-79.0871156461153));
#3645=CARTESIAN_POINT('Ctrl Pts',(-88.2882811646739,102.403958803926,-78.5394916564604));
#3646=CARTESIAN_POINT('Ctrl Pts',(-88.3237355082,101.931198710495,-78.281198278488));
#3647=CARTESIAN_POINT('Ctrl Pts',(-88.5726881997782,101.068801289506,-77.8499995679938));
#3648=CARTESIAN_POINT('Ctrl Pts',(-88.8022989313345,100.623349028228,-77.6491867686112));
#3649=CARTESIAN_POINT('Ctrl Pts',(-89.1799219644913,100.151183250598,-77.4741046930827));
#3650=CARTESIAN_POINT('Ctrl Pts',(-89.2438824969059,100.076745862652,-77.4478013653234));
#3651=CARTESIAN_POINT('Ctrl Pts',(-89.3105457858516,100.004330985068,-77.4236234448524));
#3652=CARTESIAN_POINT('',(-91.4118265169984,105.235685467738,-81.5428760182629));
#3653=CARTESIAN_POINT('Ctrl Pts',(-81.8660249138711,98.3074822374626,-71.4128027395504));
#3654=CARTESIAN_POINT('Ctrl Pts',(-82.3237270253547,98.3074822374626,-71.6770571768241));
#3655=CARTESIAN_POINT('Ctrl Pts',(-82.7726916110599,98.3818254132719,-72.0253258196487));
#3656=CARTESIAN_POINT('Ctrl Pts',(-83.5294587228727,98.6836749369366,-72.8018086256385));
#3657=CARTESIAN_POINT('Ctrl Pts',(-83.8381825657519,98.9117809702808,-73.2288909422442));
#3658=CARTESIAN_POINT('Ctrl Pts',(-84.2642108337661,99.4513482675956,-74.0139591549906));
#3659=CARTESIAN_POINT('Ctrl Pts',(-84.4147303979509,99.7982897132532,-74.427397105883));
#3660=CARTESIAN_POINT('Ctrl Pts',(-84.5187012892031,100.598975519632,-75.1573598769691));
#3661=CARTESIAN_POINT('Ctrl Pts',(-84.4719272936971,101.053974393027,-75.4725395573331));
#3662=CARTESIAN_POINT('Ctrl Pts',(-84.2144142894456,101.946025606974,-75.9185651643065));
#3663=CARTESIAN_POINT('Ctrl Pts',(-83.9900828414982,102.430163538118,-76.072953886212));
#3664=CARTESIAN_POINT('Ctrl Pts',(-83.3943596113716,103.332957803082,-76.1947311507971));
#3665=CARTESIAN_POINT('Ctrl Pts',(-83.022912997837,103.751330105905,-76.1639500741449));
#3666=CARTESIAN_POINT('Ctrl Pts',(-82.2465265160762,104.425439262707,-75.9857200884568));
#3667=CARTESIAN_POINT('Ctrl Pts',(-81.7851543098186,104.72612267149,-75.8230324929145));
#3668=CARTESIAN_POINT('Ctrl Pts',(-80.8241649502783,105.131719766025,-75.4002729960248));
#3669=CARTESIAN_POINT('Ctrl Pts',(-80.3237270253549,105.235685467738,-75.1411587919613));
#3670=CARTESIAN_POINT('Ctrl Pts',(-79.8660249138712,105.235685467738,-74.8769043546876));
#3671=CARTESIAN_POINT('Origin',(-119.078493020361,109.,-80.7499999999988));
#3672=CARTESIAN_POINT('',(-104.90435628947,98.3074822374622,-84.7139895609318));
#3673=CARTESIAN_POINT('',(-104.90435628947,98.3074822374623,-84.7139895609318));
#3674=CARTESIAN_POINT('',(-99.9488699419194,100.228885141061,-83.7562504402684));
#3675=CARTESIAN_POINT('Ctrl Pts',(-99.9488699419193,100.228885141061,-83.7562504402685));
#3676=CARTESIAN_POINT('Ctrl Pts',(-100.269274778488,99.8589135037763,-83.6332987009061));
#3677=CARTESIAN_POINT('Ctrl Pts',(-100.672060551272,99.5388009858237,-83.5687616798079));
#3678=CARTESIAN_POINT('Ctrl Pts',(-101.656557156406,98.9446450743508,-83.5546921849167));
#3679=CARTESIAN_POINT('Ctrl Pts',(-102.323796076877,98.6892023001508,-83.659021954752));
#3680=CARTESIAN_POINT('Ctrl Pts',(-103.656688844209,98.3714816818226,-84.070990296531));
#3681=CARTESIAN_POINT('Ctrl Pts',(-104.322168303632,98.3074822374624,-84.3778631705889));
#3682=CARTESIAN_POINT('Ctrl Pts',(-104.90435628947,98.3074822374624,-84.7139895609318));
#3683=CARTESIAN_POINT('',(-102.90435628947,105.235685467738,-88.1780911760691));
#3684=CARTESIAN_POINT('Ctrl Pts',(-102.90435628947,105.235685467738,-88.178091176069));
#3685=CARTESIAN_POINT('Ctrl Pts',(-102.322168303632,105.235685467738,-87.8419647857261));
#3686=CARTESIAN_POINT('Ctrl Pts',(-101.701146422792,105.145679342323,-87.4580891267805));
#3687=CARTESIAN_POINT('Ctrl Pts',(-100.583248552382,104.718635790978,-86.6737387001651));
#3688=CARTESIAN_POINT('Ctrl Pts',(-100.087436405043,104.380238803494,-86.2724890494876));
#3689=CARTESIAN_POINT('Ctrl Pts',(-99.4797157079115,103.63823946452,-85.6153691751923));
#3690=CARTESIAN_POINT('Ctrl Pts',(-99.2762414496599,103.243002384244,-85.320427254354));
#3691=CARTESIAN_POINT('Ctrl Pts',(-99.0952115751188,102.385815407921,-84.7678773474479));
#3692=CARTESIAN_POINT('Ctrl Pts',(-99.1179825761209,101.924673720388,-84.5089097354468));
#3693=CARTESIAN_POINT('Ctrl Pts',(-99.3631680629044,101.075326279613,-84.0842360150593));
#3694=CARTESIAN_POINT('Ctrl Pts',(-99.5989917777891,100.640669594177,-83.8953044405758));
#3695=CARTESIAN_POINT('Ctrl Pts',(-99.9319639746297,100.248502859387,-83.7627974003584));
#3696=CARTESIAN_POINT('Ctrl Pts',(-99.940389585881,100.238677412744,-83.7595046811735));
#3697=CARTESIAN_POINT('Ctrl Pts',(-99.9488699419193,100.228885141061,-83.7562504402685));
#3698=CARTESIAN_POINT('',(-102.90435628947,105.235685467738,-88.1780911760691));
#3699=CARTESIAN_POINT('Ctrl Pts',(-93.4118265169985,98.3074822374625,-78.0787744031257));
#3700=CARTESIAN_POINT('Ctrl Pts',(-93.9211136281798,98.3074822374625,-78.372811453861));
#3701=CARTESIAN_POINT('Ctrl Pts',(-94.4293110479316,98.3809411378057,-78.7542137874603));
#3702=CARTESIAN_POINT('Ctrl Pts',(-95.3131003585774,98.6801492903014,-79.6011997737382));
#3703=CARTESIAN_POINT('Ctrl Pts',(-95.68953602647,98.9062732240902,-80.0657700699796));
#3704=CARTESIAN_POINT('Ctrl Pts',(-96.2180755930993,99.439773757549,-80.9039616912801));
#3705=CARTESIAN_POINT('Ctrl Pts',(-96.4211158671793,99.7760817327783,-81.3392544545395));
#3706=CARTESIAN_POINT('Ctrl Pts',(-96.603988459357,100.572512615503,-82.1140272198499));
#3707=CARTESIAN_POINT('Ctrl Pts',(-96.5825452086925,101.034655609006,-82.4517288812605));
#3708=CARTESIAN_POINT('Ctrl Pts',(-96.3138784992858,101.965344390996,-82.9170732722552));
#3709=CARTESIAN_POINT('Ctrl Pts',(-96.0594130029196,102.458977333713,-83.0572595789545));
#3710=CARTESIAN_POINT('Ctrl Pts',(-95.3867915721352,103.359086193817,-83.1307566850585));
#3711=CARTESIAN_POINT('Ctrl Pts',(-94.9692620595266,103.765790736204,-83.0669701806072));
#3712=CARTESIAN_POINT('Ctrl Pts',(-94.0943036219507,104.432320373106,-82.8287936444868));
#3713=CARTESIAN_POINT('Ctrl Pts',(-93.5664254574151,104.730808636538,-82.6265294468561));
#3714=CARTESIAN_POINT('Ctrl Pts',(-92.4801710348681,105.132960205189,-82.130223321151));
#3715=CARTESIAN_POINT('Ctrl Pts',(-91.9211136281798,105.235685467738,-81.8369130689982));
#3716=CARTESIAN_POINT('Ctrl Pts',(-91.4118265169984,105.235685467738,-81.5428760182629));
#3717=CARTESIAN_POINT('Origin',(-119.078493020361,109.,-80.7499999999988));
#3718=CARTESIAN_POINT('',(-106.270002469182,105.235685467738,-90.1212479039226));
#3719=CARTESIAN_POINT('',(-106.270002469182,105.235685467738,-90.1212479039226));
#3720=CARTESIAN_POINT('Ctrl Pts',(-104.90435628947,98.3074822374624,-84.7139895609318));
#3721=CARTESIAN_POINT('Ctrl Pts',(-105.520546937821,98.3074822374624,-85.0697473976293));
#3722=CARTESIAN_POINT('Ctrl Pts',(-106.150726410955,98.3786464989181,-85.5188532090103));
#3723=CARTESIAN_POINT('Ctrl Pts',(-107.289220969567,98.6734920739597,-86.5082604731963));
#3724=CARTESIAN_POINT('Ctrl Pts',(-107.798461931632,98.8969623992174,-87.0475589280851));
#3725=CARTESIAN_POINT('Ctrl Pts',(-108.520316145588,99.4223913020677,-87.9892961628252));
#3726=CARTESIAN_POINT('Ctrl Pts',(-108.815648667087,99.7399146036544,-88.4622960553437));
#3727=CARTESIAN_POINT('Ctrl Pts',(-109.06520359177,100.328003547478,-89.1041494241911));
#3728=CARTESIAN_POINT('Ctrl Pts',(-109.116864532686,100.542611823444,-89.3070609778502));
#3729=CARTESIAN_POINT('Ctrl Pts',(-109.140178467765,101.001678002652,-89.6682684715672));
#3730=CARTESIAN_POINT('Ctrl Pts',(-109.111806983136,101.246175947599,-89.8265150985448));
#3731=CARTESIAN_POINT('Ctrl Pts',(-108.965261598155,101.753824052402,-90.080339150946));
#3732=CARTESIAN_POINT('Ctrl Pts',(-108.849954531701,102.007043208325,-90.1709510744033));
#3733=CARTESIAN_POINT('Ctrl Pts',(-108.552569635501,102.497386688197,-90.2844484102263));
#3734=CARTESIAN_POINT('Ctrl Pts',(-108.370506562727,102.734504647816,-90.3073999743598));
#3735=CARTESIAN_POINT('Ctrl Pts',(-107.75853069038,103.401878694155,-90.2932781005938));
#3736=CARTESIAN_POINT('Ctrl Pts',(-107.260215630608,103.787507531247,-90.1718542774143));
#3737=CARTESIAN_POINT('Ctrl Pts',(-106.197183712277,104.44395286517,-89.8210541610607));
#3738=CARTESIAN_POINT('Ctrl Pts',(-105.538070840598,104.739654064067,-89.5413414682492));
#3739=CARTESIAN_POINT('Ctrl Pts',(-104.200003266355,105.136149694813,-88.8976048069571));
#3740=CARTESIAN_POINT('Ctrl Pts',(-103.520546937821,105.235685467738,-88.5338490127664));
#3741=CARTESIAN_POINT('Ctrl Pts',(-102.90435628947,105.235685467738,-88.178091176069));
#3742=CARTESIAN_POINT('',(-108.270002469182,98.3074822374624,-86.6571462887851));
#3743=CARTESIAN_POINT('',(-108.270002469182,98.3074822374623,-86.6571462887851));
#3744=CARTESIAN_POINT('Ctrl Pts',(-106.270002469182,105.235685467738,-90.1212479039226));
#3745=CARTESIAN_POINT('Ctrl Pts',(-106.398364251285,105.235685467738,-90.1953576133737));
#3746=CARTESIAN_POINT('Ctrl Pts',(-106.527960736738,105.218918283964,-90.2651932010029));
#3747=CARTESIAN_POINT('Ctrl Pts',(-106.847366026658,105.139174343852,-90.425397613589));
#3748=CARTESIAN_POINT('Ctrl Pts',(-107.033287150629,105.059113530962,-90.5082215504996));
#3749=CARTESIAN_POINT('Ctrl Pts',(-107.487244640969,104.791037335221,-90.6836023495469));
#3750=CARTESIAN_POINT('Ctrl Pts',(-107.742055343965,104.569575136487,-90.7553778221103));
#3751=CARTESIAN_POINT('Ctrl Pts',(-108.312044999287,103.952474510198,-90.8506321914898));
#3752=CARTESIAN_POINT('Ctrl Pts',(-108.601687275107,103.516179693072,-90.83222067748));
#3753=CARTESIAN_POINT('Ctrl Pts',(-109.016285784176,102.748005272445,-90.6902990309755));
#3754=CARTESIAN_POINT('Ctrl Pts',(-109.166799177582,102.411600006565,-90.5937735724328));
#3755=CARTESIAN_POINT('Ctrl Pts',(-109.364309285276,101.886060973467,-90.3923049613581));
#3756=CARTESIAN_POINT('Ctrl Pts',(-109.428881856401,101.691891969437,-90.3067091143765));
#3757=CARTESIAN_POINT('Ctrl Pts',(-109.539343060738,101.309363471567,-90.1154913997023));
#3758=CARTESIAN_POINT('Ctrl Pts',(-109.58547134865,101.12019828098,-90.0094768684831));
#3759=CARTESIAN_POINT('Ctrl Pts',(-109.683806016576,100.621556930253,-89.6991065970049));
#3760=CARTESIAN_POINT('Ctrl Pts',(-109.718746169311,100.316400657043,-89.4751827475122));
#3761=CARTESIAN_POINT('Ctrl Pts',(-109.719931149862,99.6457292128168,-88.8981274115455));
#3762=CARTESIAN_POINT('Ctrl Pts',(-109.659507933391,99.2872907854466,-88.5188240602725));
#3763=CARTESIAN_POINT('Ctrl Pts',(-109.407078555524,98.8025861049536,-87.8721136642323));
#3764=CARTESIAN_POINT('Ctrl Pts',(-109.264504916411,98.6353091816041,-87.6059682053067));
#3765=CARTESIAN_POINT('Ctrl Pts',(-108.94540320403,98.4361359224893,-87.1969059803222));
#3766=CARTESIAN_POINT('Ctrl Pts',(-108.799409958408,98.3776732407719,-87.0447641078801));
#3767=CARTESIAN_POINT('Ctrl Pts',(-108.519683286228,98.3196123402596,-86.8155806823361));
#3768=CARTESIAN_POINT('Ctrl Pts',(-108.39839753492,98.3074822374624,-86.7312752145517));
#3769=CARTESIAN_POINT('Ctrl Pts',(-108.270002469182,98.3074822374624,-86.6571462887851));
#3770=CARTESIAN_POINT('Origin',(-119.078493020361,109.,-80.7499999999988));
#3771=CARTESIAN_POINT('',(-85.1260169266464,123.456832294801,-65.7663309411545));
#3772=CARTESIAN_POINT('',(-73.5607164801933,123.456832294801,-59.0891016151359));
#3773=CARTESIAN_POINT('',(-85.1260169266463,123.456832294801,-65.7663309411548));
#3774=CARTESIAN_POINT('',(-83.1162922298706,123.872941359692,-62.2368404208554));
#3775=CARTESIAN_POINT('Ctrl Pts',(-83.1162922298706,123.872941359692,-62.2368404208554));
#3776=CARTESIAN_POINT('Ctrl Pts',(-83.1062743831766,123.829770440363,-62.6116107413721));
#3777=CARTESIAN_POINT('Ctrl Pts',(-83.1509026868771,123.7792071983,-62.9828538443025));
#3778=CARTESIAN_POINT('Ctrl Pts',(-83.3664532434541,123.66173721786,-63.8135927138417));
#3779=CARTESIAN_POINT('Ctrl Pts',(-83.6030554954123,123.587986446344,-64.3071289633042));
#3780=CARTESIAN_POINT('Ctrl Pts',(-84.2623538476765,123.484750532966,-65.1560397594667));
#3781=CARTESIAN_POINT('Ctrl Pts',(-84.6849506657898,123.456832294801,-65.5116812167184));
#3782=CARTESIAN_POINT('Ctrl Pts',(-85.1260169266465,123.456832294801,-65.7663309411545));
#3783=CARTESIAN_POINT('',(-89.1260169266464,123.456832294801,-58.8381277108788));
#3784=CARTESIAN_POINT('Ctrl Pts',(-89.1260169266463,123.456832294801,-58.8381277108789));
#3785=CARTESIAN_POINT('Ctrl Pts',(-88.6849506657896,123.456832294801,-58.5834779864428));
#3786=CARTESIAN_POINT('Ctrl Pts',(-88.165657720114,123.484750532965,-58.395319135024));
#3787=CARTESIAN_POINT('Ctrl Pts',(-87.1008302289584,123.587986446343,-58.2488054113713));
#3788=CARTESIAN_POINT('Ctrl Pts',(-86.5551141732562,123.66173721786,-58.2906699753141));
#3789=CARTESIAN_POINT('Ctrl Pts',(-85.5888213740156,123.798956955934,-58.5578170932871));
#3790=CARTESIAN_POINT('Ctrl Pts',(-85.1044718647574,123.871021105468,-58.7975024013151));
#3791=CARTESIAN_POINT('Ctrl Pts',(-84.2687404142013,123.972199967385,-59.4532843052146));
#3792=CARTESIAN_POINT('Ctrl Pts',(-83.9170521365101,124.,-59.8691926348772));
#3793=CARTESIAN_POINT('Ctrl Pts',(-83.4144629487118,124.,-60.7397026434787));
#3794=CARTESIAN_POINT('Ctrl Pts',(-83.2301199084241,123.972199967385,-61.2522277910038));
#3795=CARTESIAN_POINT('Ctrl Pts',(-83.1333491468145,123.906950854201,-61.9304287037879));
#3796=CARTESIAN_POINT('Ctrl Pts',(-83.120379607442,123.890555509,-62.0839305341979));
#3797=CARTESIAN_POINT('Ctrl Pts',(-83.1162922298706,123.872941359692,-62.2368404208553));
#3798=CARTESIAN_POINT('',(-77.5607164801934,123.456832294801,-52.1608983848601));
#3799=CARTESIAN_POINT('',(-89.1260169266463,123.456832294801,-58.8381277108789));
#3800=CARTESIAN_POINT('',(-75.5607164801928,123.594519519327,-59.6249999999981));
#3801=CARTESIAN_POINT('Ctrl Pts',(-75.5607164801923,123.594519519327,-59.6249999999981));
#3802=CARTESIAN_POINT('Ctrl Pts',(-75.9177670555452,123.636893626714,-59.6249999999981));
#3803=CARTESIAN_POINT('Ctrl Pts',(-76.270167318939,123.685122421852,-59.576007942327));
#3804=CARTESIAN_POINT('Ctrl Pts',(-77.0792037993761,123.798839176147,-59.3592272707466));
#3805=CARTESIAN_POINT('Ctrl Pts',(-77.5695548504124,123.870716769224,-59.1248365924091));
#3806=CARTESIAN_POINT('Ctrl Pts',(-78.4161592503826,123.971970182233,-58.476444301003));
#3807=CARTESIAN_POINT('Ctrl Pts',(-78.7723947994248,124.,-58.0622099735219));
#3808=CARTESIAN_POINT('Ctrl Pts',(-79.2772413912376,124.,-57.1877900264742));
#3809=CARTESIAN_POINT('Ctrl Pts',(-79.4578610674346,123.971970182233,-56.672163827532));
#3810=CARTESIAN_POINT('Ctrl Pts',(-79.5960830634252,123.870716769223,-55.6147867644991));
#3811=CARTESIAN_POINT('Ctrl Pts',(-79.5538958197575,123.798839176147,-55.0729349583605));
#3812=CARTESIAN_POINT('Ctrl Pts',(-79.2949201129009,123.662988149345,-54.1064244624455));
#3813=CARTESIAN_POINT('Ctrl Pts',(-79.0605274269875,123.589960152211,-53.6161302759907));
#3814=CARTESIAN_POINT('Ctrl Pts',(-78.4121993371972,123.486046379795,-52.7696054406997));
#3815=CARTESIAN_POINT('Ctrl Pts',(-77.9980062737959,123.456832294801,-52.4133677649104));
#3816=CARTESIAN_POINT('Ctrl Pts',(-77.5607164801933,123.456832294801,-52.1608983848601));
#3817=CARTESIAN_POINT('Ctrl Pts',(-73.5607164801933,123.456832294801,-59.0891016151359));
#3818=CARTESIAN_POINT('Ctrl Pts',(-73.9980062737958,123.456832294801,-59.3415709951862));
#3819=CARTESIAN_POINT('Ctrl Pts',(-74.5136136825151,123.486046379796,-59.5221538722684));
#3820=CARTESIAN_POINT('Ctrl Pts',(-75.214498480876,123.554932441228,-59.6137729046024));
#3821=CARTESIAN_POINT('Ctrl Pts',(-75.3881510574346,123.57403977147,-59.6249999999981));
#3822=CARTESIAN_POINT('Ctrl Pts',(-75.5607164801923,123.594519519327,-59.6249999999981));
#3823=CARTESIAN_POINT('Origin',(-119.078493020361,109.,-80.7499999999988));
#3824=CARTESIAN_POINT('',(-96.6718185297735,123.456832294801,-72.4323026047302));
#3825=CARTESIAN_POINT('',(-96.6718185297736,123.456832294801,-72.4323026047302));
#3826=CARTESIAN_POINT('',(-94.4177421038261,123.892951352905,-68.5776999378933));
#3827=CARTESIAN_POINT('Ctrl Pts',(-94.4177421038264,123.892951352906,-68.5776999378912));
#3828=CARTESIAN_POINT('Ctrl Pts',(-94.3950722235507,123.847611592354,-69.0004788607279));
#3829=CARTESIAN_POINT('Ctrl Pts',(-94.4446100038828,123.791696326041,-69.4229013343407));
#3830=CARTESIAN_POINT('Ctrl Pts',(-94.6962798517419,123.665476993059,-70.3388246478844));
#3831=CARTESIAN_POINT('Ctrl Pts',(-94.9708319480395,123.588576370395,-70.867709374078));
#3832=CARTESIAN_POINT('Ctrl Pts',(-95.7182701307845,123.483657833973,-71.7750046897054));
#3833=CARTESIAN_POINT('Ctrl Pts',(-96.1902714218383,123.456832294801,-72.154281252336));
#3834=CARTESIAN_POINT('Ctrl Pts',(-96.6718185297737,123.456832294801,-72.43230260473));
#3835=CARTESIAN_POINT('',(-100.671818529773,123.456832294801,-65.5040993744542));
#3836=CARTESIAN_POINT('Ctrl Pts',(-100.671818529773,123.456832294801,-65.5040993744543));
#3837=CARTESIAN_POINT('Ctrl Pts',(-100.198890562852,123.456832294801,-65.2310542854448));
#3838=CARTESIAN_POINT('Ctrl Pts',(-99.6449352638787,123.482663841571,-65.0141879033647));
#3839=CARTESIAN_POINT('Ctrl Pts',(-98.5058533293481,123.584301615867,-64.8160574918001));
#3840=CARTESIAN_POINT('Ctrl Pts',(-97.9204236427471,123.659016564532,-64.8359793331119));
#3841=CARTESIAN_POINT('Ctrl Pts',(-96.9056954794152,123.797787553474,-65.0846768377439));
#3842=CARTESIAN_POINT('Ctrl Pts',(-96.4098673945079,123.869713255231,-65.3135356756117));
#3843=CARTESIAN_POINT('Ctrl Pts',(-95.5559638106463,123.971567821815,-65.9593477666097));
#3844=CARTESIAN_POINT('Ctrl Pts',(-95.1973252908835,124.,-66.3757915444938));
#3845=CARTESIAN_POINT('Ctrl Pts',(-94.6944496907949,124.,-67.2467976337339));
#3846=CARTESIAN_POINT('Ctrl Pts',(-94.5146381715445,123.972692167848,-67.755124974498));
#3847=CARTESIAN_POINT('Ctrl Pts',(-94.4324796442889,123.913947930132,-68.376407921987));
#3848=CARTESIAN_POINT('Ctrl Pts',(-94.4231381300388,123.903743405331,-68.4770674633497));
#3849=CARTESIAN_POINT('Ctrl Pts',(-94.4177421038264,123.892951352906,-68.5776999378912));
#3850=CARTESIAN_POINT('',(-100.671818529773,123.456832294801,-65.5040993744543));
#3851=CARTESIAN_POINT('Ctrl Pts',(-85.1260169266465,123.456832294801,-65.7663309411545));
#3852=CARTESIAN_POINT('Ctrl Pts',(-85.5837190381301,123.456832294801,-66.0305853784282));
#3853=CARTESIAN_POINT('Ctrl Pts',(-86.122720562641,123.486454820705,-66.2229054686833));
#3854=CARTESIAN_POINT('Ctrl Pts',(-87.2307450620227,123.590202391576,-66.3909926328699));
#3855=CARTESIAN_POINT('Ctrl Pts',(-87.7998683754043,123.662779767014,-66.3670498363015));
#3856=CARTESIAN_POINT('Ctrl Pts',(-88.8096922981326,123.797321626501,-66.140954313845));
#3857=CARTESIAN_POINT('Ctrl Pts',(-89.3225329048017,123.868752483667,-65.9268338105032));
#3858=CARTESIAN_POINT('Ctrl Pts',(-90.208346563904,123.970860942253,-65.3026051841426));
#3859=CARTESIAN_POINT('Ctrl Pts',(-90.5808483157038,124.,-64.8915779677916));
#3860=CARTESIAN_POINT('Ctrl Pts',(-91.095874324207,124.,-63.9995267538447));
#3861=CARTESIAN_POINT('Ctrl Pts',(-91.2655834593138,123.970860942253,-63.4714171656563));
#3862=CARTESIAN_POINT('Ctrl Pts',(-91.3632744779603,123.868752483666,-62.3921657206742));
#3863=CARTESIAN_POINT('Ctrl Pts',(-91.2922879699909,123.797321626501,-61.8409724755356));
#3864=CARTESIAN_POINT('Ctrl Pts',(-90.9831804747559,123.662779767014,-60.8533915438754));
#3865=CARTESIAN_POINT('Ctrl Pts',(-90.7193538881309,123.590202391575,-60.3485448983168));
#3866=CARTESIAN_POINT('Ctrl Pts',(-90.0197738842044,123.486454820704,-59.47301111593));
#3867=CARTESIAN_POINT('Ctrl Pts',(-89.5837190381299,123.456832294801,-59.1023821481526));
#3868=CARTESIAN_POINT('Ctrl Pts',(-89.1260169266463,123.456832294801,-58.8381277108788));
#3869=CARTESIAN_POINT('Origin',(-119.078493020361,109.,-80.7499999999988));
#3870=CARTESIAN_POINT('',(-108.164348302245,123.456832294801,-79.0675177625366));
#3871=CARTESIAN_POINT('',(-108.164348302245,123.456832294801,-79.0675177625365));
#3872=CARTESIAN_POINT('',(-105.277091391218,123.923615035047,-74.5275001761057));
#3873=CARTESIAN_POINT('Ctrl Pts',(-105.277091391218,123.923615035047,-74.5275001761056));
#3874=CARTESIAN_POINT('Ctrl Pts',(-105.275365738248,123.921622422635,-74.5492158639596));
#3875=CARTESIAN_POINT('Ctrl Pts',(-105.273837242761,123.919598892701,-74.5709499461767));
#3876=CARTESIAN_POINT('Ctrl Pts',(-105.238853605271,123.865658954398,-75.1423248070353));
#3877=CARTESIAN_POINT('Ctrl Pts',(-105.33860750079,123.794453706366,-75.701175262549));
#3878=CARTESIAN_POINT('Ctrl Pts',(-105.746737061739,123.654133883405,-76.7806745481755));
#3879=CARTESIAN_POINT('Ctrl Pts',(-106.120272716169,123.5787523934,-77.3509626000236));
#3880=CARTESIAN_POINT('Ctrl Pts',(-107.054281271328,123.479989785222,-78.3346823431572));
#3881=CARTESIAN_POINT('Ctrl Pts',(-107.613395871184,123.456832294801,-78.7494252281526));
#3882=CARTESIAN_POINT('Ctrl Pts',(-108.164348302246,123.456832294801,-79.0675177625365));
#3883=CARTESIAN_POINT('',(-112.164348302245,123.456832294801,-72.1393145322606));
#3884=CARTESIAN_POINT('Ctrl Pts',(-112.164348302245,123.456832294801,-72.1393145322606));
#3885=CARTESIAN_POINT('Ctrl Pts',(-111.613395871184,123.456832294801,-71.8212219978767));
#3886=CARTESIAN_POINT('Ctrl Pts',(-110.974660696811,123.479989785221,-71.5443859932717));
#3887=CARTESIAN_POINT('Ctrl Pts',(-109.655730131473,123.578752393399,-71.2273707287195));
#3888=CARTESIAN_POINT('Ctrl Pts',(-108.975078363883,123.654133883405,-71.1890233886878));
#3889=CARTESIAN_POINT('Ctrl Pts',(-107.836139778689,123.794453706366,-71.3753224636836));
#3890=CARTESIAN_POINT('Ctrl Pts',(-107.302284139538,123.865658954397,-71.5683582837951));
#3891=CARTESIAN_POINT('Ctrl Pts',(-106.383953947217,123.96943271423,-72.1762726463728));
#3892=CARTESIAN_POINT('Ctrl Pts',(-105.998960269092,124.,-72.5907067654734));
#3893=CARTESIAN_POINT('Ctrl Pts',(-105.482985495051,124.,-73.4844012895352));
#3894=CARTESIAN_POINT('Ctrl Pts',(-105.318978111356,123.971981653342,-74.0003959692113));
#3895=CARTESIAN_POINT('Ctrl Pts',(-105.277091391218,123.923615035047,-74.5275001761056));
#3896=CARTESIAN_POINT('',(-112.164348302245,123.456832294801,-72.1393145322605));
#3897=CARTESIAN_POINT('Ctrl Pts',(-96.6718185297737,123.456832294801,-72.43230260473));
#3898=CARTESIAN_POINT('Ctrl Pts',(-97.2080109095617,123.456832294801,-72.741873419538));
#3899=CARTESIAN_POINT('Ctrl Pts',(-97.8378331599511,123.489300624785,-72.9756291788421));
#3900=CARTESIAN_POINT('Ctrl Pts',(-99.1346770015159,123.601479985038,-73.210267194341));
#3901=CARTESIAN_POINT('Ctrl Pts',(-99.801733680399,123.679673134231,-73.2116784585455));
#3902=CARTESIAN_POINT('Ctrl Pts',(-100.899904621245,123.812998388381,-73.0077930813484));
#3903=CARTESIAN_POINT('Ctrl Pts',(-101.417162434113,123.877803175384,-72.8258148556167));
#3904=CARTESIAN_POINT('Ctrl Pts',(-102.313026843884,123.972069837582,-72.2590940486296));
#3905=CARTESIAN_POINT('Ctrl Pts',(-102.69054002654,124.,-71.8723715243807));
#3906=CARTESIAN_POINT('Ctrl Pts',(-103.196264738206,124.,-70.9964306291323));
#3907=CARTESIAN_POINT('Ctrl Pts',(-103.342419677093,123.972069837582,-70.4761333605637));
#3908=CARTESIAN_POINT('Ctrl Pts',(-103.385282087912,123.877803175384,-69.4169316198625));
#3909=CARTESIAN_POINT('Ctrl Pts',(-103.284250947897,123.812998388381,-68.8779841007473));
#3910=CARTESIAN_POINT('Ctrl Pts',(-102.911735393587,123.67967313423,-67.8249974796778));
#3911=CARTESIAN_POINT('Ctrl Pts',(-102.576984863492,123.601479985038,-67.2480150821033));
#3912=CARTESIAN_POINT('Ctrl Pts',(-101.725360460594,123.489300624784,-66.2422343783163));
#3913=CARTESIAN_POINT('Ctrl Pts',(-101.208010909561,123.456832294801,-65.8136701892623));
#3914=CARTESIAN_POINT('Ctrl Pts',(-100.671818529773,123.456832294801,-65.5040993744543));
#3915=CARTESIAN_POINT('Origin',(-119.078493020361,109.,-80.7499999999988));
#3916=CARTESIAN_POINT('',(-115.529994481957,123.456832294801,-74.0824712601142));
#3917=CARTESIAN_POINT('',(-115.529994481957,123.456832294801,-74.082471260114));
#3918=CARTESIAN_POINT('Ctrl Pts',(-108.164348302246,123.456832294801,-79.0675177625365));
#3919=CARTESIAN_POINT('Ctrl Pts',(-108.844463055017,123.456832294801,-79.4601821981288));
#3920=CARTESIAN_POINT('Ctrl Pts',(-109.637912977074,123.491441900927,-79.7804741154724));
#3921=CARTESIAN_POINT('Ctrl Pts',(-111.275183810088,123.611693066724,-80.170706138189));
#3922=CARTESIAN_POINT('Ctrl Pts',(-112.118571906507,123.696010228407,-80.2428658921871));
#3923=CARTESIAN_POINT('Ctrl Pts',(-113.398550856209,123.828649318389,-80.1045968599479));
#3924=CARTESIAN_POINT('Ctrl Pts',(-113.937605814753,123.885984825864,-79.974373351834));
#3925=CARTESIAN_POINT('Ctrl Pts',(-114.643393821985,123.950735654834,-79.6153146748024));
#3926=CARTESIAN_POINT('Ctrl Pts',(-114.862132214305,123.968740024147,-79.4686771786292));
#3927=CARTESIAN_POINT('Ctrl Pts',(-115.243722739859,123.993392806363,-79.1229603686417));
#3928=CARTESIAN_POINT('Ctrl Pts',(-115.406496999395,124.,-78.9237921724865));
#3929=CARTESIAN_POINT('Ctrl Pts',(-115.660952638663,124.,-78.4830620770019));
#3930=CARTESIAN_POINT('Ctrl Pts',(-115.752050226392,123.993392806363,-78.2425113350836));
#3931=CARTESIAN_POINT('Ctrl Pts',(-115.860654503579,123.968740024147,-77.7391858411162));
#3932=CARTESIAN_POINT('Ctrl Pts',(-115.878277104252,123.950735654834,-77.4764340884979));
#3933=CARTESIAN_POINT('Ctrl Pts',(-115.836337036395,123.885984825864,-76.6856744060329));
#3934=CARTESIAN_POINT('Ctrl Pts',(-115.679586423319,123.828649318388,-76.1537273638406));
#3935=CARTESIAN_POINT('Ctrl Pts',(-115.159341442944,123.696010228406,-74.9760985609694));
#3936=CARTESIAN_POINT('Ctrl Pts',(-114.675155214641,123.611693066724,-74.2817829212208));
#3937=CARTESIAN_POINT('Ctrl Pts',(-113.518568953091,123.491441900926,-73.0589807983134));
#3938=CARTESIAN_POINT('Ctrl Pts',(-112.844463055016,123.456832294801,-72.531978967853));
#3939=CARTESIAN_POINT('Ctrl Pts',(-112.164348302245,123.456832294801,-72.1393145322606));
#3940=CARTESIAN_POINT('',(-111.529994481957,123.456832294801,-81.0106744903897));
#3941=CARTESIAN_POINT('',(-111.529994481957,123.456832294801,-81.0106744903897));
#3942=CARTESIAN_POINT('Ctrl Pts',(-115.529994481957,123.456832294801,-74.0824712601142));
#3943=CARTESIAN_POINT('Ctrl Pts',(-115.65835626406,123.456832294801,-74.1565809695654));
#3944=CARTESIAN_POINT('Ctrl Pts',(-115.77745320865,123.461475653088,-74.2446022954246));
#3945=CARTESIAN_POINT('Ctrl Pts',(-116.046607194207,123.483194384997,-74.4918445203156));
#3946=CARTESIAN_POINT('Ctrl Pts',(-116.181936272838,123.504836535895,-74.6622964502142));
#3947=CARTESIAN_POINT('Ctrl Pts',(-116.463492476953,123.573840873615,-75.1362850362945));
#3948=CARTESIAN_POINT('Ctrl Pts',(-116.573472758241,123.62806730643,-75.4589141577373));
#3949=CARTESIAN_POINT('Ctrl Pts',(-116.724373411066,123.761245635907,-76.2800519723337));
#3950=CARTESIAN_POINT('Ctrl Pts',(-116.704520006728,123.840165624527,-76.7977027010819));
#3951=CARTESIAN_POINT('Ctrl Pts',(-116.53883398008,123.93828517935,-77.6608633532843));
#3952=CARTESIAN_POINT('Ctrl Pts',(-116.424541973442,123.968919507233,-78.0229943017362));
#3953=CARTESIAN_POINT('Ctrl Pts',(-116.189563012637,123.995063180093,-78.5706187310189));
#3954=CARTESIAN_POINT('Ctrl Pts',(-116.090247091074,123.99999005338,-78.7688860801498));
#3955=CARTESIAN_POINT('Ctrl Pts',(-115.86944609645,124.000009911765,-79.1514313247033));
#3956=CARTESIAN_POINT('Ctrl Pts',(-115.74750688821,123.995107474062,-79.3365182359193));
#3957=CARTESIAN_POINT('Ctrl Pts',(-115.391456612351,123.969070285569,-79.8131657732718));
#3958=CARTESIAN_POINT('Ctrl Pts',(-115.135714858818,123.938576005114,-80.0927177542768));
#3959=CARTESIAN_POINT('Ctrl Pts',(-114.471237782264,123.840607113622,-80.6686229218872));
#3960=CARTESIAN_POINT('Ctrl Pts',(-114.031900126614,123.761512834073,-80.9456186309926));
#3961=CARTESIAN_POINT('Ctrl Pts',(-113.24419775823,123.628137504237,-81.2260282504464));
#3962=CARTESIAN_POINT('Ctrl Pts',(-112.909789654842,123.573903068408,-81.292149830288));
#3963=CARTESIAN_POINT('Ctrl Pts',(-112.358412824606,123.504868123884,-81.2853999107625));
#3964=CARTESIAN_POINT('Ctrl Pts',(-112.143032917437,123.483209990156,-81.2534392614886));
#3965=CARTESIAN_POINT('Ctrl Pts',(-111.794203638433,123.461478073366,-81.1439450618975));
#3966=CARTESIAN_POINT('Ctrl Pts',(-111.658389547695,123.456832294801,-81.0848034161563));
#3967=CARTESIAN_POINT('Ctrl Pts',(-111.529994481957,123.456832294801,-81.0106744903897));
#3968=CARTESIAN_POINT('Origin',(-119.078493020361,109.,-80.7499999999988));
#3969=CARTESIAN_POINT('',(-126.564449609913,108.0824948189,-67.7839428436388));
#3970=CARTESIAN_POINT('',(-122.424179917669,122.42480974691,-74.9551003076436));
#3971=CARTESIAN_POINT('Origin',(-119.078493020361,109.,-80.7499999999988));
#3972=CARTESIAN_POINT('',(-77.2010015942,108.0824948189,-39.2839428436393));
#3973=CARTESIAN_POINT('',(-126.564449609913,108.0824948189,-67.7839428436388));
#3974=CARTESIAN_POINT('',(-73.0607319019557,122.42480974691,-46.4551003076441));
#3975=CARTESIAN_POINT('Origin',(-69.7150450046476,109.,-52.2499999999992));
#3976=CARTESIAN_POINT('',(-122.424179917669,122.42480974691,-74.9551003076436));
#3977=CARTESIAN_POINT('Origin',(-69.7150450046476,109.,-52.2499999999992));
#3978=CARTESIAN_POINT('',(-73.7335498795933,101.937180526609,-39.2897453861299));
#3979=CARTESIAN_POINT('',(-70.2694482644555,101.937180526609,-37.2897453861299));
#3980=CARTESIAN_POINT('',(-73.7335498795933,101.937180526609,-39.2897453861299));
#3981=CARTESIAN_POINT('',(-67.366968793295,123.991664350565,-50.3169872981059));
#3982=CARTESIAN_POINT('Origin',(-67.1169687932943,109.,-50.7499999999993));
#3983=CARTESIAN_POINT('',(-63.9028671781572,123.991664350565,-48.3169872981059));
#3984=CARTESIAN_POINT('',(-67.366968793295,123.991664350565,-50.3169872981059));
#3985=CARTESIAN_POINT('Origin',(-63.6528671781565,109.,-48.7499999999993));
#3986=CARTESIAN_POINT('Origin',(-69.7150450046476,109.,-52.2499999999992));
#3987=CARTESIAN_POINT('',(-78.2150450046475,109.,-37.5275681356637));
#3988=CARTESIAN_POINT('Origin',(-69.7150450046476,109.,-52.2499999999992));
#3989=CARTESIAN_POINT('',(-76.9580463854329,108.363035329266,-39.7047536091873));
#3990=CARTESIAN_POINT('',(-76.9580463854329,108.363035329266,-39.7047536091873));
#3991=CARTESIAN_POINT('',(-73.6123594881249,96.7732359445554,-45.4996533015424));
#3992=CARTESIAN_POINT('Origin',(-69.7150450046476,109.,-52.2499999999992));
#3993=CARTESIAN_POINT('',(-73.6123594881249,96.7732359445554,-45.4996533015424));
#3994=CARTESIAN_POINT('',(-65.8177305211704,96.7732359445554,-59.0003466984559));
#3995=CARTESIAN_POINT('',(-65.8177305211704,96.7732359445554,-59.0003466984559));
#3996=CARTESIAN_POINT('',(-62.4720436238624,108.363035329266,-64.7952463908111));
#3997=CARTESIAN_POINT('Origin',(-69.7150450046476,109.,-52.2499999999992));
#3998=CARTESIAN_POINT('',(-62.4720436238624,108.363035329266,-64.7952463908111));
#3999=CARTESIAN_POINT('',(-66.3693581073396,121.863728726179,-58.0448996923544));
#4000=CARTESIAN_POINT('',(-66.3693581073396,121.863728726179,-58.0448996923544));
#4001=CARTESIAN_POINT('',(-73.0607319019557,121.863728726179,-46.4551003076441));
#4002=CARTESIAN_POINT('Origin',(-69.7150450046476,109.,-52.2499999999992));
#4003=CARTESIAN_POINT('',(-73.0607319019557,121.863728726179,-46.4551003076441));
#4004=CARTESIAN_POINT('Origin',(-63.6528671781565,109.,-48.7499999999993));
#4005=CARTESIAN_POINT('',(-72.1528671781564,109.,-34.0275681356638));
#4006=CARTESIAN_POINT('Origin',(-63.6528671781565,109.,-48.7499999999993));
#4007=CARTESIAN_POINT('',(-56.6032733899647,101.437180526611,-60.9602546138697));
#4008=CARTESIAN_POINT('',(-56.6032733899647,101.437180526611,-60.9602546138697));
#4009=CARTESIAN_POINT('',(-56.8532733899647,100.571155122826,-60.5272419119775));
#4010=CARTESIAN_POINT('',(-56.8532733899647,100.571155122826,-60.5272419119775));
#4011=CARTESIAN_POINT('',(-57.2862860918569,101.071155122826,-59.7772419119775));
#4012=CARTESIAN_POINT('',(-70.4524609663477,100.571155122824,-36.9727580880222));
#4013=CARTESIAN_POINT('',(-70.4524609663477,100.571155122824,-36.9727580880222));
#4014=CARTESIAN_POINT('',(-70.7024609663477,101.437180526609,-36.5397453861299));
#4015=CARTESIAN_POINT('',(-70.7024609663477,101.437180526609,-36.53974538613));
#4016=CARTESIAN_POINT('',(-70.2694482644555,101.937180526609,-37.2897453861299));
#4017=CARTESIAN_POINT('',(-63.9028671781572,124.991664350565,-48.3169872981059));
#4018=CARTESIAN_POINT('',(-63.9028671781572,124.991664350565,-48.3169872981059));
#4019=CARTESIAN_POINT('',(-63.4028671781572,124.991664350565,-49.1830127018903));
#4020=CARTESIAN_POINT('',(-63.4028671781572,124.991664350565,-49.1830127018903));
#4021=CARTESIAN_POINT('',(-63.4028671781572,123.991664350565,-49.1830127018903));
#4022=CARTESIAN_POINT('Origin',(-69.7150450046476,109.,-52.2499999999992));
#4023=CARTESIAN_POINT('',(-78.2150450046475,109.,-37.5275681356637));
#4024=CARTESIAN_POINT('Origin',(-67.1169687932943,109.,-50.7499999999993));
#4025=CARTESIAN_POINT('',(-60.3173750051025,100.571155122826,-62.5272419119774));
#4026=CARTESIAN_POINT('',(-60.7503877069946,101.071155122826,-61.7772419119775));
#4027=CARTESIAN_POINT('',(-60.0673750051025,101.437180526611,-62.9602546138697));
#4028=CARTESIAN_POINT('',(-60.3173750051025,100.571155122826,-62.5272419119774));
#4029=CARTESIAN_POINT('',(-60.0673750051025,101.437180526611,-62.9602546138697));
#4030=CARTESIAN_POINT('',(-66.866968793295,124.991664350565,-51.1830127018903));
#4031=CARTESIAN_POINT('',(-66.866968793295,123.991664350565,-51.1830127018903));
#4032=CARTESIAN_POINT('',(-67.366968793295,124.991664350565,-50.3169872981059));
#4033=CARTESIAN_POINT('',(-66.866968793295,124.991664350565,-51.1830127018903));
#4034=CARTESIAN_POINT('',(-67.366968793295,124.991664350565,-50.3169872981059));
#4035=CARTESIAN_POINT('',(-74.1665625814855,101.437180526609,-38.5397453861299));
#4036=CARTESIAN_POINT('',(-73.7335498795933,101.937180526609,-39.2897453861299));
#4037=CARTESIAN_POINT('',(-73.9165625814855,100.571155122824,-38.9727580880221));
#4038=CARTESIAN_POINT('',(-74.1665625814855,101.437180526609,-38.5397453861299));
#4039=CARTESIAN_POINT('',(-73.9165625814855,100.571155122824,-38.9727580880221));
#4040=CARTESIAN_POINT('',(-73.616968793294,109.,-39.4916697508017));
#4041=CARTESIAN_POINT('Origin',(-67.116968793295,109.,-50.7499999999981));
#4042=CARTESIAN_POINT('Origin',(-119.078493020361,109.,-80.7499999999988));
#4043=CARTESIAN_POINT('',(-122.975807503838,96.7732359445554,-73.9996533015419));
#4044=CARTESIAN_POINT('',(-122.975807503838,96.7732359445554,-73.9996533015419));
#4045=CARTESIAN_POINT('',(-126.321494401146,108.363035329266,-68.2047536091869));
#4046=CARTESIAN_POINT('Origin',(-119.078493020361,109.,-80.7499999999988));
#4047=CARTESIAN_POINT('',(-126.564449609913,108.0824948189,-67.7839428436388));
#4048=CARTESIAN_POINT('',(-122.424179917669,121.863728726179,-74.9551003076436));
#4049=CARTESIAN_POINT('',(-122.424179917669,121.863728726179,-74.9551003076436));
#4050=CARTESIAN_POINT('',(-115.732806123053,121.863728726179,-86.5448996923539));
#4051=CARTESIAN_POINT('Origin',(-119.078493020361,109.,-80.7499999999988));
#4052=CARTESIAN_POINT('',(-115.732806123053,122.42480974691,-86.5448996923539));
#4053=CARTESIAN_POINT('',(-111.835491639576,108.363035329266,-93.2952463908107));
#4054=CARTESIAN_POINT('',(-111.835491639576,108.363035329266,-93.2952463908107));
#4055=CARTESIAN_POINT('',(-115.181178536884,96.7732359445553,-87.5003466984555));
#4056=CARTESIAN_POINT('Origin',(-119.078493020361,109.,-80.7499999999988));
#4057=CARTESIAN_POINT('',(-114.938223328117,96.49269543419,-87.9211574640035));
#4058=CARTESIAN_POINT('Origin',(-75.5607164801933,129.,-55.624999999998));
#4059=CARTESIAN_POINT('',(-75.5607164801933,129.,-59.6249999999981));
#4060=CARTESIAN_POINT('Origin',(-75.5607164801933,129.,-55.624999999998));
#4061=CARTESIAN_POINT('',(-75.5607164801933,129.,-59.1249999999981));
#4062=CARTESIAN_POINT('Origin',(-75.5607164801933,129.,-55.624999999998));
#4063=CARTESIAN_POINT('Origin',(-75.5607164801933,-5.00102499999999,-55.624999999998));
#4064=CARTESIAN_POINT('',(-75.5607164801933,-5.00102499999999,-59.6249999999981));
#4065=CARTESIAN_POINT('',(-77.5607164801934,122.937359864766,-52.1608983848606));
#4066=CARTESIAN_POINT('',(-77.5607164801934,122.937359864766,-52.1608983848601));
#4067=CARTESIAN_POINT('',(-73.5607164801933,122.937359864767,-59.0891016151359));
#4068=CARTESIAN_POINT('Ctrl Pts',(-77.5607164801933,122.937359864766,-52.1608983848601));
#4069=CARTESIAN_POINT('Ctrl Pts',(-77.1232537523542,122.937359864766,-51.9083291611818));
#4070=CARTESIAN_POINT('Ctrl Pts',(-76.60754249421,122.967689419789,-51.7277743724565));
#4071=CARTESIAN_POINT('Ctrl Pts',(-75.5502948880754,123.075440885261,-51.5896430799529));
#4072=CARTESIAN_POINT('Ctrl Pts',(-75.008612000326,123.151115999848,-51.6318312278756));
#4073=CARTESIAN_POINT('Ctrl Pts',(-74.0423701006026,123.291794528869,-51.8907349645996));
#4074=CARTESIAN_POINT('Ctrl Pts',(-73.5520995881099,123.366192507349,-52.1250380084307));
#4075=CARTESIAN_POINT('Ctrl Pts',(-72.7054703736856,123.47098799846,-52.7733608760245));
#4076=CARTESIAN_POINT('Ctrl Pts',(-72.3491310307417,123.5,-53.1876291712969));
#4077=CARTESIAN_POINT('Ctrl Pts',(-71.8440986993692,123.5,-54.0623708286991));
#4078=CARTESIAN_POINT('Ctrl Pts',(-71.6635015031528,123.47098799846,-54.5781038996925));
#4079=CARTESIAN_POINT('Ctrl Pts',(-71.5253520371743,123.366192507349,-55.635467740767));
#4080=CARTESIAN_POINT('Ctrl Pts',(-71.5675749052789,123.29179452887,-56.1772059812275));
#4081=CARTESIAN_POINT('Ctrl Pts',(-71.826478642003,123.151115999849,-57.143447880951));
#4082=CARTESIAN_POINT('Ctrl Pts',(-72.060784078038,123.075440885262,-57.6336530964987));
#4083=CARTESIAN_POINT('Ctrl Pts',(-72.709033089471,122.96768941979,-58.4801907352497));
#4084=CARTESIAN_POINT('Ctrl Pts',(-73.1232537523542,122.937359864767,-58.8365323914576));
#4085=CARTESIAN_POINT('Ctrl Pts',(-73.5607164801933,122.937359864767,-59.0891016151359));
#4086=CARTESIAN_POINT('',(-73.5607164801933,122.937359864767,-59.0891016151359));
#4087=CARTESIAN_POINT('Origin',(-88.2037045535141,128.101020514434,-62.924432567491));
#4088=CARTESIAN_POINT('',(-84.3072367627289,129.005199011952,-62.924432567491));
#4089=CARTESIAN_POINT('Origin',(-88.2037045535141,128.101020514434,-62.924432567491));
#4090=CARTESIAN_POINT('',(-84.7942952365771,128.892176699762,-62.9244325674911));
#4091=CARTESIAN_POINT('Origin',(-88.2037045535141,128.101020514434,-62.9244325674911));
#4092=CARTESIAN_POINT('Origin',(-39.9537393796627,-79.8274313593171,-35.0673021859779));
#4093=CARTESIAN_POINT('',(-36.0572715888775,-78.9232528617992,-35.0673021859779));
#4094=CARTESIAN_POINT('Origin',(-100.711351574804,127.535898384862,-70.1457259421618));
#4095=CARTESIAN_POINT('',(-97.1336428108046,129.324752766862,-70.1457259421618));
#4096=CARTESIAN_POINT('Origin',(-100.711351574804,127.535898384862,-70.1457259421618));
#4097=CARTESIAN_POINT('',(-97.5808564063047,129.101145969112,-70.1457259421618));
#4098=CARTESIAN_POINT('Origin',(-100.711351574804,127.535898384862,-70.1457259421618));
#4099=CARTESIAN_POINT('Origin',(24.6400845185815,-123.166973801907,2.2259594296606));
#4100=CARTESIAN_POINT('',(28.2177932825812,-121.378119419907,2.2259594296606));
#4101=CARTESIAN_POINT('Origin',(-113.529994481957,127.343145750508,-77.5465728752519));
#4102=CARTESIAN_POINT('',(-110.506278697883,129.96176043334,-77.5465728752519));
#4103=CARTESIAN_POINT('Origin',(-113.529994481957,127.343145750508,-77.5465728752519));
#4104=CARTESIAN_POINT('',(-110.884243170892,129.634433597986,-77.5465728752519));
#4105=CARTESIAN_POINT('Origin',(-113.529994481957,127.343145750508,-77.5465728752519));
#4106=CARTESIAN_POINT('Origin',(101.486213576105,-120.9361854544,46.5930927272026));
#4107=CARTESIAN_POINT('',(104.509929360179,-118.317570771568,46.5930927272026));
#4108=CARTESIAN_POINT('Origin',(-75.5607164801933,126.,-55.624999999998));
#4109=CARTESIAN_POINT('',(-75.5607164801933,126.,-59.1249999999981));
#4110=CARTESIAN_POINT('Origin',(-75.5607164801933,126.,-55.624999999998));
#4111=CARTESIAN_POINT('',(-75.5607164801933,126.,-58.4249999999981));
#4112=CARTESIAN_POINT('Origin',(-75.5607164801933,126.,-55.624999999998));
#4113=CARTESIAN_POINT('Origin',(-75.5607164801933,126.,-55.624999999998));
#4114=CARTESIAN_POINT('',(-75.5607164801933,126.,-59.1249999999981));
#4115=CARTESIAN_POINT('Origin',(-87.531272949388,125.203243035567,-62.5362039998373));
#4116=CARTESIAN_POINT('',(-84.121863632451,125.994399220895,-62.5362039998373));
#4117=CARTESIAN_POINT('Origin',(-87.531272949388,125.203243035567,-62.5362039998373));
#4118=CARTESIAN_POINT('',(-84.8037454958384,125.836167983829,-62.5362039998373));
#4119=CARTESIAN_POINT('Origin',(-87.531272949388,125.203243035567,-62.5362039998373));
#4120=CARTESIAN_POINT('Origin',(-87.531272949388,125.203243035567,-62.5362039998373));
#4121=CARTESIAN_POINT('',(-84.121863632451,125.994399220895,-62.5362039998373));
#4122=CARTESIAN_POINT('Origin',(-99.4123134691276,124.937822173509,-69.3957259421618));
#4123=CARTESIAN_POINT('',(-96.281818300628,126.503069757759,-69.3957259421618));
#4124=CARTESIAN_POINT('Origin',(-99.4123134691276,124.937822173509,-69.3957259421618));
#4125=CARTESIAN_POINT('',(-96.907917334328,126.190020240909,-69.3957259421618));
#4126=CARTESIAN_POINT('Origin',(-99.4123134691276,124.937822173509,-69.3957259421618));
#4127=CARTESIAN_POINT('Origin',(-99.4123134691276,124.937822173509,-69.3957259421618));
#4128=CARTESIAN_POINT('',(-96.281818300628,126.503069757759,-69.3957259421618));
#4129=CARTESIAN_POINT('Origin',(-147.457758061401,109.,-97.1347763108453));
#4130=CARTESIAN_POINT('',(-122.114391405223,109.,-67.4916697508013));
#4131=CARTESIAN_POINT('Origin',(-115.614391405224,109.,-78.7499999999976));
#4132=CARTESIAN_POINT('',(-153.9577580614,109.,-85.8764460616489));
#4133=CARTESIAN_POINT('',(-117.386134507203,101.605059126311,-67.4270749801284));
#4134=CARTESIAN_POINT('',(-111.565481622863,103.438089404292,-62.8444992851723));
#4135=CARTESIAN_POINT('Ctrl Pts',(-117.386134507204,101.60505912631,-67.4270749801283));
#4136=CARTESIAN_POINT('Ctrl Pts',(-117.384843998764,101.603815224188,-67.4273233385933));
#4137=CARTESIAN_POINT('Ctrl Pts',(-117.383552105126,101.602572260028,-67.4275705183945));
#4138=CARTESIAN_POINT('Ctrl Pts',(-117.105783250958,101.335811456963,-67.4804062339256));
#4139=CARTESIAN_POINT('Ctrl Pts',(-116.763727423833,101.113949509274,-67.4772489203251));
#4140=CARTESIAN_POINT('Ctrl Pts',(-115.970697123411,100.70633252813,-67.3909870285613));
#4141=CARTESIAN_POINT('Ctrl Pts',(-115.446738163493,100.524469125477,-67.2695400568307));
#4142=CARTESIAN_POINT('Ctrl Pts',(-114.405674258994,100.28486436115,-66.9123137382068));
#4143=CARTESIAN_POINT('Ctrl Pts',(-113.888815670701,100.22768844038,-66.6754382808512));
#4144=CARTESIAN_POINT('Ctrl Pts',(-113.435498258322,100.22768844038,-66.413715350786));
#4145=CARTESIAN_POINT('Ctrl Pts',(-113.045853744828,100.22768844038,-66.1887539860318));
#4146=CARTESIAN_POINT('Ctrl Pts',(-112.64222922698,100.270378061999,-65.9097091373666));
#4147=CARTESIAN_POINT('Ctrl Pts',(-111.934430306435,100.476843984392,-65.2895980494646));
#4148=CARTESIAN_POINT('Ctrl Pts',(-111.630654997402,100.641526829723,-64.9483785209879));
#4149=CARTESIAN_POINT('Ctrl Pts',(-111.2369795781,101.04252635731,-64.3493295404366));
#4150=CARTESIAN_POINT('Ctrl Pts',(-111.099937593526,101.284167988039,-64.0558123049316));
#4151=CARTESIAN_POINT('Ctrl Pts',(-110.986598478824,101.851747702853,-63.5337079966479));
#4152=CARTESIAN_POINT('Ctrl Pts',(-111.009713416376,102.178321465582,-63.3059402798856));
#4153=CARTESIAN_POINT('Ctrl Pts',(-111.191412176548,102.807744434161,-62.9912287955964));
#4154=CARTESIAN_POINT('Ctrl Pts',(-111.351088823113,103.136138059265,-62.8857591987216));
#4155=CARTESIAN_POINT('Ctrl Pts',(-111.565481622863,103.438089404292,-62.8444992851724));
#4156=CARTESIAN_POINT('Ctrl Pts',(-111.565481622863,103.438089404292,-62.8444992851724));
#4157=CARTESIAN_POINT('Ctrl Pts',(-111.575188933326,103.451761204159,-62.8426311124026));
#4158=CARTESIAN_POINT('Ctrl Pts',(-111.585003582125,103.465381199048,-62.8408869585381));
#4159=CARTESIAN_POINT('Ctrl Pts',(-111.823912628857,103.792091077249,-62.8018507603263));
#4160=CARTESIAN_POINT('Ctrl Pts',(-112.112006606371,104.073708899229,-62.8337382694769));
#4161=CARTESIAN_POINT('Ctrl Pts',(-112.759808395975,104.553028941455,-62.9926274651217));
#4162=CARTESIAN_POINT('Ctrl Pts',(-113.170797750173,104.759746443146,-63.1481468200871));
#4163=CARTESIAN_POINT('Ctrl Pts',(-114.013782161377,105.021576797287,-63.5341097697223));
#4164=CARTESIAN_POINT('Ctrl Pts',(-114.445853744829,105.077430701572,-63.7638828554352));
#4165=CARTESIAN_POINT('Ctrl Pts',(-115.288815670702,105.077430701572,-64.2505671502546));
#4166=CARTESIAN_POINT('Ctrl Pts',(-115.767594076423,105.002693000391,-64.5533994185862));
#4167=CARTESIAN_POINT('Ctrl Pts',(-116.652114853179,104.700016463066,-65.1817663880356));
#4168=CARTESIAN_POINT('Ctrl Pts',(-117.058123820432,104.473289105623,-65.5075087398144));
#4169=CARTESIAN_POINT('Ctrl Pts',(-117.59419825037,103.990784840806,-66.0388312545589));
#4170=CARTESIAN_POINT('Ctrl Pts',(-117.798111636135,103.73410733426,-66.281258295277));
#4171=CARTESIAN_POINT('Ctrl Pts',(-117.971447315925,103.296228661322,-66.6204521442011));
#4172=CARTESIAN_POINT('Ctrl Pts',(-118.007599536035,103.14149423203,-66.7297304001928));
#4173=CARTESIAN_POINT('Ctrl Pts',(-118.025761966741,102.824004944285,-66.9316462349407));
#4174=CARTESIAN_POINT('Ctrl Pts',(-118.007691799887,102.661241838733,-67.0242780679549));
#4175=CARTESIAN_POINT('Ctrl Pts',(-117.914598780889,102.338758161266,-67.1855199066884));
#4176=CARTESIAN_POINT('Ctrl Pts',(-117.839876304636,102.180078121956,-67.2536096461054));
#4177=CARTESIAN_POINT('Ctrl Pts',(-117.643713131067,101.879175318306,-67.3610917996573));
#4178=CARTESIAN_POINT('Ctrl Pts',(-117.522786130607,101.736775618063,-67.4007763629426));
#4179=CARTESIAN_POINT('Ctrl Pts',(-117.386134507204,101.60505912631,-67.4270749801282));
#4180=CARTESIAN_POINT('',(-106.165171981646,103.438089404295,-86.8623521842208));
#4181=CARTESIAN_POINT('',(-100.344519097302,101.605059126314,-82.2797764892636));
#4182=CARTESIAN_POINT('Ctrl Pts',(-106.165171981646,103.438089404295,-86.862352184219));
#4183=CARTESIAN_POINT('Ctrl Pts',(-106.14419730415,103.462308875692,-86.8634802540479));
#4184=CARTESIAN_POINT('Ctrl Pts',(-106.12282827633,103.486302635371,-86.8641514184887));
#4185=CARTESIAN_POINT('Ctrl Pts',(-105.818714172361,103.818683816975,-86.8673779259697));
#4186=CARTESIAN_POINT('Ctrl Pts',(-105.472391325601,104.085740432872,-86.7940722130298));
#4187=CARTESIAN_POINT('Ctrl Pts',(-104.731279077633,104.539153956812,-86.5696833263198));
#4188=CARTESIAN_POINT('Ctrl Pts',(-104.271314809741,104.741671619492,-86.3849512882693));
#4189=CARTESIAN_POINT('Ctrl Pts',(-103.33961664048,105.01118751589,-85.9511255373707));
#4190=CARTESIAN_POINT('Ctrl Pts',(-102.867626486497,105.077430701576,-85.7021134546504));
#4191=CARTESIAN_POINT('Ctrl Pts',(-102.441408937237,105.077430701576,-85.4560366378519));
#4192=CARTESIAN_POINT('Ctrl Pts',(-102.014157839508,105.077430701576,-85.2093631015665));
#4193=CARTESIAN_POINT('Ctrl Pts',(-101.56105927878,105.010210941309,-84.9242504184528));
#4194=CARTESIAN_POINT('Ctrl Pts',(-100.752419784988,104.696117862631,-84.3353138424256));
#4195=CARTESIAN_POINT('Ctrl Pts',(-100.397371710978,104.448780822016,-84.0310608152941));
#4196=CARTESIAN_POINT('Ctrl Pts',(-99.9882037851011,103.92339933994,-83.5499074785033));
#4197=CARTESIAN_POINT('Ctrl Pts',(-99.8584603905707,103.660815277971,-83.3448119619325));
#4198=CARTESIAN_POINT('Ctrl Pts',(-99.7452298798465,103.091082457567,-82.9637606339507));
#4199=CARTESIAN_POINT('Ctrl Pts',(-99.7621917782077,102.784236407494,-82.7872192164191));
#4200=CARTESIAN_POINT('Ctrl Pts',(-99.9262957445862,102.215763592511,-82.502982808928));
#4201=CARTESIAN_POINT('Ctrl Pts',(-100.082544658828,101.922589786887,-82.379514298611));
#4202=CARTESIAN_POINT('Ctrl Pts',(-100.312341841756,101.642706629092,-82.2911817419664));
#4203=CARTESIAN_POINT('Ctrl Pts',(-100.328291840436,101.623796748554,-82.2853723510623));
#4204=CARTESIAN_POINT('Ctrl Pts',(-100.344519097301,101.605059126315,-82.2797764892642));
#4205=CARTESIAN_POINT('Ctrl Pts',(-100.344519097301,101.605059126315,-82.2797764892642));
#4206=CARTESIAN_POINT('Ctrl Pts',(-100.550215520806,101.367541355351,-82.2088434432281));
#4207=CARTESIAN_POINT('Ctrl Pts',(-100.802602048525,101.15899254472,-82.1740857015096));
#4208=CARTESIAN_POINT('Ctrl Pts',(-101.47214666584,100.72565116497,-82.1694959867722));
#4209=CARTESIAN_POINT('Ctrl Pts',(-101.955786523501,100.527533200142,-82.2510215111824));
#4210=CARTESIAN_POINT('Ctrl Pts',(-102.926860882229,100.278935400847,-82.5586126482226));
#4211=CARTESIAN_POINT('Ctrl Pts',(-103.414157839508,100.227688440382,-82.784491970971));
#4212=CARTESIAN_POINT('Ctrl Pts',(-104.267626486497,100.227688440382,-83.2772423240549));
#4213=CARTESIAN_POINT('Ctrl Pts',(-104.705846427788,100.278428703028,-83.5847461309404));
#4214=CARTESIAN_POINT('Ctrl Pts',(-105.498304549662,100.491254479672,-84.2597427183605));
#4215=CARTESIAN_POINT('Ctrl Pts',(-105.853076223232,100.653134652889,-84.6266736743588));
#4216=CARTESIAN_POINT('Ctrl Pts',(-106.353797244182,101.032460766724,-85.2674323799564));
#4217=CARTESIAN_POINT('Ctrl Pts',(-106.557061980701,101.260971981571,-85.5885220082683));
#4218=CARTESIAN_POINT('Ctrl Pts',(-106.72625467127,101.679226130855,-86.024626674228));
#4219=CARTESIAN_POINT('Ctrl Pts',(-106.760576424903,101.831187432809,-86.1626137356242));
#4220=CARTESIAN_POINT('Ctrl Pts',(-106.774196861679,102.153837950614,-86.4089088160002));
#4221=CARTESIAN_POINT('Ctrl Pts',(-106.753460724005,102.324558208363,-86.5171780914983));
#4222=CARTESIAN_POINT('Ctrl Pts',(-106.652169358375,102.675441791642,-86.692619883138));
#4223=CARTESIAN_POINT('Ctrl Pts',(-106.572948453007,102.850982888141,-86.7574812847633));
#4224=CARTESIAN_POINT('Ctrl Pts',(-106.38376792248,103.164953280743,-86.8360360636708));
#4225=CARTESIAN_POINT('Ctrl Pts',(-106.28046465974,103.304960886828,-86.8561514599566));
#4226=CARTESIAN_POINT('Ctrl Pts',(-106.165171981646,103.438089404295,-86.862352184219));
#4227=CARTESIAN_POINT('',(-105.707515158216,101.445788778226,-60.813667453584));
#4228=CARTESIAN_POINT('',(-101.324821922316,103.6146594521,-56.8374045514775));
#4229=CARTESIAN_POINT('Ctrl Pts',(-105.707515158216,101.445788778225,-60.8136674535836));
#4230=CARTESIAN_POINT('Ctrl Pts',(-105.483577684551,101.227887906321,-60.8640309956986));
#4231=CARTESIAN_POINT('Ctrl Pts',(-105.222582053125,101.039304544329,-60.8807352012508));
#4232=CARTESIAN_POINT('Ctrl Pts',(-104.602960841079,100.67854055414,-60.8556299182567));
#4233=CARTESIAN_POINT('Ctrl Pts',(-104.1892589951,100.508020898325,-60.7865580098289));
#4234=CARTESIAN_POINT('Ctrl Pts',(-103.362197532696,100.282687776782,-60.5388045693685));
#4235=CARTESIAN_POINT('Ctrl Pts',(-102.949106981883,100.22768844038,-60.359394524506));
#4236=CARTESIAN_POINT('Ctrl Pts',(-102.587887471937,100.22768844038,-60.1508443432025));
#4237=CARTESIAN_POINT('Ctrl Pts',(-102.254878013721,100.22768844038,-59.9585812428588));
#4238=CARTESIAN_POINT('Ctrl Pts',(-101.918162195562,100.275039954704,-59.7132182406853));
#4239=CARTESIAN_POINT('Ctrl Pts',(-101.348088424631,100.488116881772,-59.166211609912));
#4240=CARTESIAN_POINT('Ctrl Pts',(-101.114826914581,100.65473625473,-58.8648160959221));
#4241=CARTESIAN_POINT('Ctrl Pts',(-100.809047976543,101.052694817512,-58.3193334032543));
#4242=CARTESIAN_POINT('Ctrl Pts',(-100.708587237918,101.302215526292,-58.04101395854));
#4243=CARTESIAN_POINT('Ctrl Pts',(-100.646124764096,101.871223563749,-57.5488477901271));
#4244=CARTESIAN_POINT('Ctrl Pts',(-100.683391349424,102.19108472861,-57.3355266127738));
#4245=CARTESIAN_POINT('Ctrl Pts',(-100.861743664517,102.808915271389,-57.0266113413844));
#4246=CARTESIAN_POINT('Ctrl Pts',(-101.013824739271,103.144973641637,-56.9119727511829));
#4247=CARTESIAN_POINT('Ctrl Pts',(-101.251985600091,103.511086021696,-56.8502538040771));
#4248=CARTESIAN_POINT('Ctrl Pts',(-101.287761408094,103.563290529642,-56.8430050519095));
#4249=CARTESIAN_POINT('Ctrl Pts',(-101.324821922315,103.614659452099,-56.8374045514776));
#4250=CARTESIAN_POINT('Ctrl Pts',(-101.324821922315,103.614659452099,-56.8374045514776));
#4251=CARTESIAN_POINT('Ctrl Pts',(-101.507571534895,103.867965453781,-56.8097878465912));
#4252=CARTESIAN_POINT('Ctrl Pts',(-101.722903603191,104.100150075329,-56.8237200261498));
#4253=CARTESIAN_POINT('Ctrl Pts',(-102.23560907329,104.537239540928,-56.9235644528227));
#4254=CARTESIAN_POINT('Ctrl Pts',(-102.577115242381,104.745590666186,-57.0374747177044));
#4255=CARTESIAN_POINT('Ctrl Pts',(-103.286625217418,105.015534918971,-57.3429707585513));
#4256=CARTESIAN_POINT('Ctrl Pts',(-103.654878013722,105.077430701572,-57.5337101122621));
#4257=CARTESIAN_POINT('Ctrl Pts',(-104.349106981883,105.077430701572,-57.9345233939092));
#4258=CARTESIAN_POINT('Ctrl Pts',(-104.725589216724,105.005615111484,-58.1773409020166));
#4259=CARTESIAN_POINT('Ctrl Pts',(-105.40533608587,104.720635512592,-58.6802507026948));
#4260=CARTESIAN_POINT('Ctrl Pts',(-105.708442531058,104.5080414619,-58.9408794643765));
#4261=CARTESIAN_POINT('Ctrl Pts',(-106.134628803274,104.039966782051,-59.3986735814598));
#4262=CARTESIAN_POINT('Ctrl Pts',(-106.301658407902,103.762601478164,-59.628755601445));
#4263=CARTESIAN_POINT('Ctrl Pts',(-106.466981515918,103.150363245665,-60.0574871392715));
#4264=CARTESIAN_POINT('Ctrl Pts',(-106.463597321879,102.815336528851,-60.256562220115));
#4265=CARTESIAN_POINT('Ctrl Pts',(-106.281537692062,102.184663471148,-60.5718987489666));
#4266=CARTESIAN_POINT('Ctrl Pts',(-106.096327018674,101.866378403104,-60.6994795605523));
#4267=CARTESIAN_POINT('Ctrl Pts',(-105.801011946827,101.53963142162,-60.790807331965));
#4268=CARTESIAN_POINT('Ctrl Pts',(-105.755075673419,101.492067221763,-60.8029710928037));
#4269=CARTESIAN_POINT('Ctrl Pts',(-105.707515158216,101.445788778225,-60.8136674535836));
#4270=CARTESIAN_POINT('',(-94.501534612098,103.614659452104,-80.2229951080884));
#4271=CARTESIAN_POINT('',(-90.1188413761952,101.445788778232,-76.2467322059816));
#4272=CARTESIAN_POINT('Ctrl Pts',(-94.5015346120983,103.614659452105,-80.222995108087));
#4273=CARTESIAN_POINT('Ctrl Pts',(-94.2999319259417,103.85835031517,-80.2346736634614));
#4274=CARTESIAN_POINT('Ctrl Pts',(-94.0660003649607,104.078184573876,-80.204501523942));
#4275=CARTESIAN_POINT('Ctrl Pts',(-93.506215357663,104.508041461903,-80.0757568941915));
#4276=CARTESIAN_POINT('Ctrl Pts',(-93.1289510064958,104.720635512595,-79.9435733934488));
#4277=CARTESIAN_POINT('Ctrl Pts',(-92.353544908723,105.005615111488,-79.6063502369639));
#4278=CARTESIAN_POINT('Ctrl Pts',(-91.9550176607982,105.077430701576,-79.4017158115723));
#4279=CARTESIAN_POINT('Ctrl Pts',(-91.5937981508529,105.077430701576,-79.1931656302689));
#4280=CARTESIAN_POINT('Ctrl Pts',(-91.2445310553966,105.077430701576,-78.9915161786881));
#4281=CARTESIAN_POINT('Ctrl Pts',(-90.8794457263923,105.009294935457,-78.75672916701));
#4282=CARTESIAN_POINT('Ctrl Pts',(-90.2394279750154,104.71379978534,-78.2726325195484));
#4283=CARTESIAN_POINT('Ctrl Pts',(-89.9651725619102,104.486205632632,-78.0225716794456));
#4284=CARTESIAN_POINT('Ctrl Pts',(-89.615152325688,103.992202355958,-77.5948073108704));
#4285=CARTESIAN_POINT('Ctrl Pts',(-89.4966157452444,103.711875068197,-77.3893068873646));
#4286=CARTESIAN_POINT('Ctrl Pts',(-89.4038756583846,103.11192693574,-77.0059525649689));
#4287=CARTESIAN_POINT('Ctrl Pts',(-89.4297352858526,102.792723417415,-76.8274306857825));
#4288=CARTESIAN_POINT('Ctrl Pts',(-89.5987392296941,102.207276582589,-76.5347072683697));
#4289=CARTESIAN_POINT('Ctrl Pts',(-89.7529823542094,101.902585866878,-76.4012820305381));
#4290=CARTESIAN_POINT('Ctrl Pts',(-90.0135013341837,101.566233275656,-76.2843454877329));
#4291=CARTESIAN_POINT('Ctrl Pts',(-90.0649390949408,101.505064596095,-76.2644831614807));
#4292=CARTESIAN_POINT('Ctrl Pts',(-90.1188413761922,101.445788778236,-76.2467322059833));
#4293=CARTESIAN_POINT('Ctrl Pts',(-90.1188413761922,101.445788778236,-76.2467322059833));
#4294=CARTESIAN_POINT('Ctrl Pts',(-90.3002565105157,101.246288307949,-76.1869890578052));
#4295=CARTESIAN_POINT('Ctrl Pts',(-90.5105127919593,101.068816696773,-76.1519939958911));
#4296=CARTESIAN_POINT('Ctrl Pts',(-91.0593017712658,100.696030871333,-76.1274842987972));
#4297=CARTESIAN_POINT('Ctrl Pts',(-91.4519661767371,100.513444242339,-76.1724547480489));
#4298=CARTESIAN_POINT('Ctrl Pts',(-92.2447448611874,100.279759997467,-76.3919616980159));
#4299=CARTESIAN_POINT('Ctrl Pts',(-92.6445310553966,100.227688440383,-76.5666450480926));
#4300=CARTESIAN_POINT('Ctrl Pts',(-93.3550176607982,100.227688440383,-76.9768446809768));
#4301=CARTESIAN_POINT('Ctrl Pts',(-93.7169365927499,100.282687776784,-77.2448865696132));
#4302=CARTESIAN_POINT('Ctrl Pts',(-94.3450280972656,100.508020898327,-77.8372660863158));
#4303=CARTESIAN_POINT('Ctrl Pts',(-94.6116970476415,100.678540554143,-78.1610064403122));
#4304=CARTESIAN_POINT('Ctrl Pts',(-94.9727271872904,101.071379412638,-78.7316542894256));
#4305=CARTESIAN_POINT('Ctrl Pts',(-95.1064606462321,101.310297639174,-79.0194069254365));
#4306=CARTESIAN_POINT('Ctrl Pts',(-95.2231499598568,101.866378403107,-79.5323746661135));
#4307=CARTESIAN_POINT('Ctrl Pts',(-95.2052670726821,102.184663471151,-79.7565622201121));
#4308=CARTESIAN_POINT('Ctrl Pts',(-95.0232074428643,102.815336528854,-80.0718987489636));
#4309=CARTESIAN_POINT('Ctrl Pts',(-94.8524954626127,103.150363245668,-80.174367087394));
#4310=CARTESIAN_POINT('Ctrl Pts',(-94.5857570770073,103.510107742139,-80.2161985863255));
#4311=CARTESIAN_POINT('Ctrl Pts',(-94.5443515978532,103.562903652559,-80.2205147813183));
#4312=CARTESIAN_POINT('Ctrl Pts',(-94.5015346120983,103.614659452105,-80.222995108087));
#4313=CARTESIAN_POINT('',(-94.2209929096256,101.354811290699,-54.2576156201439));
#4314=CARTESIAN_POINT('',(-90.5178421019398,103.716919354992,-50.5448617949466));
#4315=CARTESIAN_POINT('Ctrl Pts',(-94.2209929096261,101.354811290699,-54.2576156201434));
#4316=CARTESIAN_POINT('Ctrl Pts',(-94.0304505856294,101.165865871972,-54.3062458592498));
#4317=CARTESIAN_POINT('Ctrl Pts',(-93.8147279386984,100.999081132478,-54.3308652529223));
#4318=CARTESIAN_POINT('Ctrl Pts',(-93.2853347608051,100.664686636251,-54.335231850713));
#4319=CARTESIAN_POINT('Ctrl Pts',(-92.9240531847944,100.499668449628,-54.2909952556545));
#4320=CARTESIAN_POINT('Ctrl Pts',(-92.1976667058189,100.281331189612,-54.0944571890166));
#4321=CARTESIAN_POINT('Ctrl Pts',(-91.8328571384615,100.22768844038,-53.9414246850278));
#4322=CARTESIAN_POINT('Ctrl Pts',(-91.5141993333915,100.22768844038,-53.7574475154913));
#4323=CARTESIAN_POINT('Ctrl Pts',(-91.1998056536407,100.22768844038,-53.5759322398556));
#4324=CARTESIAN_POINT('Ctrl Pts',(-90.8886903708508,100.280334555034,-53.3396967948896));
#4325=CARTESIAN_POINT('Ctrl Pts',(-90.3733823362884,100.504055421459,-52.8139276391242));
#4326=CARTESIAN_POINT('Ctrl Pts',(-90.1688519647511,100.67573731595,-52.5249835715961));
#4327=CARTESIAN_POINT('Ctrl Pts',(-89.9037680431757,101.07557755986,-52.0026890248464));
#4328=CARTESIAN_POINT('Ctrl Pts',(-89.8203132445372,101.325643828305,-51.7350194741849));
#4329=CARTESIAN_POINT('Ctrl Pts',(-89.7787639540569,101.887795138889,-51.2622217134503));
#4330=CARTESIAN_POINT('Ctrl Pts',(-89.8201747804601,102.200227598979,-51.0575503555047));
#4331=CARTESIAN_POINT('Ctrl Pts',(-89.9932484568848,102.799772401019,-50.7577779544845));
#4332=CARTESIAN_POINT('Ctrl Pts',(-90.1366138563365,103.127423563352,-50.6424075012184));
#4333=CARTESIAN_POINT('Ctrl Pts',(-90.3868899039983,103.531966317969,-50.5657018885759));
#4334=CARTESIAN_POINT('Ctrl Pts',(-90.4505284239739,103.625948972014,-50.5527189917843));
#4335=CARTESIAN_POINT('Ctrl Pts',(-90.5178421019398,103.716919354992,-50.5448617949466));
#4336=CARTESIAN_POINT('Ctrl Pts',(-90.5178421019398,103.716919354992,-50.5448617949466));
#4337=CARTESIAN_POINT('Ctrl Pts',(-90.6677586076694,103.919522486378,-50.5273627734945));
#4338=CARTESIAN_POINT('Ctrl Pts',(-90.8363800498654,104.106877932436,-50.5357972502939));
#4339=CARTESIAN_POINT('Ctrl Pts',(-91.2761732604758,104.511610804944,-50.6070468270981));
#4340=CARTESIAN_POINT('Ctrl Pts',(-91.5920360022583,104.725595554037,-50.7031575728346));
#4341=CARTESIAN_POINT('Ctrl Pts',(-92.2536368706955,105.008647929721,-50.9755401075456));
#4342=CARTESIAN_POINT('Ctrl Pts',(-92.5998056536411,105.077430701572,-51.1510611092587));
#4343=CARTESIAN_POINT('Ctrl Pts',(-93.232857138462,105.077430701572,-51.5165535544309));
#4344=CARTESIAN_POINT('Ctrl Pts',(-93.5619700271323,105.00741652851,-51.7314145195672));
#4345=CARTESIAN_POINT('Ctrl Pts',(-94.1455671289826,104.731116876602,-52.1752710421669));
#4346=CARTESIAN_POINT('Ctrl Pts',(-94.3998110409153,104.525345718212,-52.4049023097321));
#4347=CARTESIAN_POINT('Ctrl Pts',(-94.768377540354,104.0613168212,-52.8259509372149));
#4348=CARTESIAN_POINT('Ctrl Pts',(-94.9105232806575,103.7725092302,-53.0468145506106));
#4349=CARTESIAN_POINT('Ctrl Pts',(-95.0354212815802,103.14720818058,-53.4590643079669));
#4350=CARTESIAN_POINT('Ctrl Pts',(-95.0172814114049,102.810893242388,-53.6509908389482));
#4351=CARTESIAN_POINT('Ctrl Pts',(-94.8377871142222,102.18910675761,-53.9618840813374));
#4352=CARTESIAN_POINT('Ctrl Pts',(-94.66647754768,101.869149596082,-54.0980936002161));
#4353=CARTESIAN_POINT('Ctrl Pts',(-94.365959399355,101.505588017214,-54.2160961273275));
#4354=CARTESIAN_POINT('Ctrl Pts',(-94.2953494579818,101.428544668509,-54.238638331267));
#4355=CARTESIAN_POINT('Ctrl Pts',(-94.2209929096261,101.354811290699,-54.2576156201434));
#4356=CARTESIAN_POINT('',(-83.0247832218288,103.716919354995,-73.6500196516034));
#4357=CARTESIAN_POINT('',(-79.3216324141422,101.354811290702,-69.9372658264059));
#4358=CARTESIAN_POINT('Ctrl Pts',(-83.0247832218292,103.716919354995,-73.6500196516021));
#4359=CARTESIAN_POINT('Ctrl Pts',(-82.8561874835582,103.929460895585,-73.6618384029087));
#4360=CARTESIAN_POINT('Ctrl Pts',(-82.6660644120803,104.123947093647,-73.6439402061671));
#4361=CARTESIAN_POINT('Ctrl Pts',(-82.1939330584629,104.523769595123,-73.5508930043753));
#4362=CARTESIAN_POINT('Ctrl Pts',(-81.8675496354975,104.73010984644,-73.445550762439));
#4363=CARTESIAN_POINT('Ctrl Pts',(-81.1904340361545,105.007198663853,-73.1618575252943));
#4364=CARTESIAN_POINT('Ctrl Pts',(-80.8392691645201,105.077430701576,-72.9840354250022));
#4365=CARTESIAN_POINT('Ctrl Pts',(-80.5201100123077,105.077430701576,-72.799768802558));
#4366=CARTESIAN_POINT('Ctrl Pts',(-80.2107074631239,105.077430701576,-72.6211351574988));
#4367=CARTESIAN_POINT('Ctrl Pts',(-79.8902928105569,105.010817414927,-72.4125520697033));
#4368=CARTESIAN_POINT('Ctrl Pts',(-79.3296459208272,104.735983399352,-71.9826313276384));
#4369=CARTESIAN_POINT('Ctrl Pts',(-79.0898300656876,104.528017888669,-71.760587957699));
#4370=CARTESIAN_POINT('Ctrl Pts',(-78.7510680657571,104.056494164301,-71.353383279585));
#4371=CARTESIAN_POINT('Ctrl Pts',(-78.6282785579301,103.763711210128,-71.1414137376349));
#4372=CARTESIAN_POINT('Ctrl Pts',(-78.5328756547392,103.137634877854,-70.745080894813));
#4373=CARTESIAN_POINT('Ctrl Pts',(-78.5604078289852,102.804749283705,-70.5600387968433));
#4374=CARTESIAN_POINT('Ctrl Pts',(-78.7363549099663,102.1952507163,-70.2552895131407));
#4375=CARTESIAN_POINT('Ctrl Pts',(-78.8964707374473,101.878104564589,-70.1153157381806));
#4376=CARTESIAN_POINT('Ctrl Pts',(-79.1804605765672,101.511189981574,-69.9855724361914));
#4377=CARTESIAN_POINT('Ctrl Pts',(-79.2490780626133,101.431324815456,-69.9596178450133));
#4378=CARTESIAN_POINT('Ctrl Pts',(-79.3216324141422,101.354811290702,-69.9372658264059));
#4379=CARTESIAN_POINT('Ctrl Pts',(-79.3216324141422,101.354811290702,-69.9372658264059));
#4380=CARTESIAN_POINT('Ctrl Pts',(-79.4994951487113,101.167242875335,-69.8824711646265));
#4381=CARTESIAN_POINT('Ctrl Pts',(-79.7016131069151,101.000214480644,-69.8498916678611));
#4382=CARTESIAN_POINT('Ctrl Pts',(-80.2057230797504,100.662451096332,-69.8278045615312));
#4383=CARTESIAN_POINT('Ctrl Pts',(-80.5536874604562,100.495779124926,-69.8625291904263));
#4384=CARTESIAN_POINT('Ctrl Pts',(-81.2563406796862,100.27868878512,-70.0464877548005));
#4385=CARTESIAN_POINT('Ctrl Pts',(-81.6107074631236,100.227688440383,-70.1962640269031));
#4386=CARTESIAN_POINT('Ctrl Pts',(-82.2392691645199,100.227688440383,-70.5591642944065));
#4387=CARTESIAN_POINT('Ctrl Pts',(-82.5546266768382,100.281496733901,-70.7990065603189));
#4388=CARTESIAN_POINT('Ctrl Pts',(-83.0885412363331,100.500470869914,-71.330731274177));
#4389=CARTESIAN_POINT('Ctrl Pts',(-83.3075860460983,100.665962481951,-71.6219894477902));
#4390=CARTESIAN_POINT('Ctrl Pts',(-83.6098374691532,101.054698410516,-72.1567503717173));
#4391=CARTESIAN_POINT('Ctrl Pts',(-83.7166215744316,101.303006298545,-72.4375565865388));
#4392=CARTESIAN_POINT('Ctrl Pts',(-83.7911705443989,101.870113330836,-72.9351916366745));
#4393=CARTESIAN_POINT('Ctrl Pts',(-83.7588055350932,102.189611224737,-73.1512430725076));
#4394=CARTESIAN_POINT('Ctrl Pts',(-83.5796024921405,102.810388775268,-73.4616318477727));
#4395=CARTESIAN_POINT('Ctrl Pts',(-83.4227987210069,103.14619075922,-73.5732303508662));
#4396=CARTESIAN_POINT('Ctrl Pts',(-83.1543827768569,103.546695163547,-73.6361875753525));
#4397=CARTESIAN_POINT('Ctrl Pts',(-83.0912106178557,103.633177136873,-73.6453630162586));
#4398=CARTESIAN_POINT('Ctrl Pts',(-83.0247832218292,103.716919354995,-73.6500196516021));
#4399=CARTESIAN_POINT('',(-79.2724338250639,100.514077983564,-46.3961169753473));
#4400=CARTESIAN_POINT('',(-82.9097405209592,104.714077983563,-45.6961169753459));
#4401=CARTESIAN_POINT('Ctrl Pts',(-79.2724338250643,100.514077983563,-46.3961169753468));
#4402=CARTESIAN_POINT('Ctrl Pts',(-79.1265511423845,100.610404906306,-46.2160498567682));
#4403=CARTESIAN_POINT('Ctrl Pts',(-79.0063377502804,100.729412390803,-46.0312428512855));
#4404=CARTESIAN_POINT('Ctrl Pts',(-78.7783882480642,101.056823805357,-45.5960981587349));
#4405=CARTESIAN_POINT('Ctrl Pts',(-78.6879980806413,101.308592332844,-45.3220312346838));
#4406=CARTESIAN_POINT('Ctrl Pts',(-78.637346637553,101.87720020589,-44.8375673373119));
#4407=CARTESIAN_POINT('Ctrl Pts',(-78.6768221832288,102.194506798829,-44.627746600585));
#4408=CARTESIAN_POINT('Ctrl Pts',(-78.8531987651598,102.805493201169,-44.3222533994151));
#4409=CARTESIAN_POINT('Ctrl Pts',(-79.001482969892,103.138605462875,-44.2068647088189));
#4410=CARTESIAN_POINT('Ctrl Pts',(-79.3969069246043,103.764324604201,-44.094165099005));
#4411=CARTESIAN_POINT('Ctrl Pts',(-79.6443545210792,104.056618970362,-44.0962005762319));
#4412=CARTESIAN_POINT('Ctrl Pts',(-80.1647562293486,104.52433820779,-44.1867417540882));
#4413=CARTESIAN_POINT('Ctrl Pts',(-80.4728761101798,104.731264722065,-44.2812762970742));
#4414=CARTESIAN_POINT('Ctrl Pts',(-81.1163900166925,105.008060588784,-44.5457120366282));
#4415=CARTESIAN_POINT('Ctrl Pts',(-81.4522447708355,105.077430701572,-44.7150138327633));
#4416=CARTESIAN_POINT('Ctrl Pts',(-82.0632775106341,105.077430701572,-45.0677937495697));
#4417=CARTESIAN_POINT('Ctrl Pts',(-82.3778245440648,105.008060588784,-45.2740016005717));
#4418=CARTESIAN_POINT('Ctrl Pts',(-82.7431217757092,104.824474558593,-45.5559387185791));
#4419=CARTESIAN_POINT('Ctrl Pts',(-82.8290587463787,104.772275635182,-45.6260680866036));
#4420=CARTESIAN_POINT('Ctrl Pts',(-82.9097405209591,104.714077983563,-45.6961169753458));
#4421=CARTESIAN_POINT('Ctrl Pts',(-82.9097405209591,104.714077983563,-45.6961169753458));
#4422=CARTESIAN_POINT('Ctrl Pts',(-83.0761634408585,104.594033237844,-45.8406073594606));
#4423=CARTESIAN_POINT('Ctrl Pts',(-83.2198007296756,104.447978167203,-45.9848429857255));
#4424=CARTESIAN_POINT('Ctrl Pts',(-83.5031306358671,104.056618970362,-46.3240660048471));
#4425=CARTESIAN_POINT('Ctrl Pts',(-83.6286172090919,103.764324604201,-46.5373441708864));
#4426=CARTESIAN_POINT('Ctrl Pts',(-83.7287284613526,103.138605462875,-46.936141165839));
#4427=CARTESIAN_POINT('Ctrl Pts',(-83.7029410263529,102.805493201169,-47.1222533994152));
#4428=CARTESIAN_POINT('Ctrl Pts',(-83.5265644444219,102.194506798829,-47.427746600585));
#4429=CARTESIAN_POINT('Ctrl Pts',(-83.3645921290135,101.87720020589,-47.5668437943321));
#4430=CARTESIAN_POINT('Ctrl Pts',(-82.9197083651289,101.308592332844,-47.7652103065652));
#4431=CARTESIAN_POINT('Ctrl Pts',(-82.6371643628521,101.056823805357,-47.8239635873502));
#4432=CARTESIAN_POINT('Ctrl Pts',(-82.0505767043741,100.665529520269,-47.8480598380025));
#4433=CARTESIAN_POINT('Ctrl Pts',(-81.7069979829943,100.499547348265,-47.8149418084238));
#4434=CARTESIAN_POINT('Ctrl Pts',(-81.0131896142114,100.280826524207,-47.637618632861));
#4435=CARTESIAN_POINT('Ctrl Pts',(-80.6632775106336,100.227688440379,-47.4926648801669));
#4436=CARTESIAN_POINT('Ctrl Pts',(-80.3577611407344,100.227688440379,-47.3162749217637));
#4437=CARTESIAN_POINT('Ctrl Pts',(-80.0522447708351,100.227688440379,-47.1398849633606));
#4438=CARTESIAN_POINT('Ctrl Pts',(-79.7517550868392,100.280826524207,-46.9093290689175));
#4439=CARTESIAN_POINT('Ctrl Pts',(-79.4198158701761,100.42589403654,-46.5696141741228));
#4440=CARTESIAN_POINT('Ctrl Pts',(-79.3431576996741,100.467378724402,-46.4834134527748));
#4441=CARTESIAN_POINT('Ctrl Pts',(-79.2724338250643,100.514077983563,-46.3961169753468));
#4442=CARTESIAN_POINT('',(-68.2116924394259,104.714077983566,-65.5538830246524));
#4443=CARTESIAN_POINT('',(-71.8489991353209,100.514077983566,-64.8538830246516));
#4444=CARTESIAN_POINT('Ctrl Pts',(-68.2116924394265,104.714077983567,-65.5538830246511));
#4445=CARTESIAN_POINT('Ctrl Pts',(-68.0452695195272,104.594033237848,-65.4093926405365));
#4446=CARTESIAN_POINT('Ctrl Pts',(-67.9016322307103,104.447978167207,-65.2651570142717));
#4447=CARTESIAN_POINT('Ctrl Pts',(-67.6183023245187,104.056618970366,-64.9259339951503));
#4448=CARTESIAN_POINT('Ctrl Pts',(-67.4928157512939,103.764324604205,-64.7126558291111));
#4449=CARTESIAN_POINT('Ctrl Pts',(-67.3927044990331,103.138605462879,-64.3138588341587));
#4450=CARTESIAN_POINT('Ctrl Pts',(-67.4184919340327,102.805493201172,-64.1277466005826));
#4451=CARTESIAN_POINT('Ctrl Pts',(-67.5948685159636,102.194506798833,-63.8222533994129));
#4452=CARTESIAN_POINT('Ctrl Pts',(-67.7568408313719,101.877200205893,-63.683156205666));
#4453=CARTESIAN_POINT('Ctrl Pts',(-68.2017245952565,101.308592332847,-63.484789693433));
#4454=CARTESIAN_POINT('Ctrl Pts',(-68.4842685975332,101.056823805361,-63.4260364126481));
#4455=CARTESIAN_POINT('Ctrl Pts',(-69.0708562560112,100.665529520272,-63.4019401619959));
#4456=CARTESIAN_POINT('Ctrl Pts',(-69.4144349773908,100.499547348269,-63.4350581915746));
#4457=CARTESIAN_POINT('Ctrl Pts',(-70.1082433461736,100.28082652421,-63.6123813671375));
#4458=CARTESIAN_POINT('Ctrl Pts',(-70.4581554497515,100.227688440383,-63.7573351198316));
#4459=CARTESIAN_POINT('Ctrl Pts',(-71.0691881895501,100.227688440383,-64.110115036638));
#4460=CARTESIAN_POINT('Ctrl Pts',(-71.369677873546,100.28082652421,-64.340670931081));
#4461=CARTESIAN_POINT('Ctrl Pts',(-71.701617090209,100.425894036543,-64.6803858258755));
#4462=CARTESIAN_POINT('Ctrl Pts',(-71.7782752607111,100.467378724405,-64.7665865472236));
#4463=CARTESIAN_POINT('Ctrl Pts',(-71.8489991353208,100.514077983566,-64.8538830246515));
#4464=CARTESIAN_POINT('Ctrl Pts',(-71.8489991353208,100.514077983566,-64.8538830246515));
#4465=CARTESIAN_POINT('Ctrl Pts',(-71.9948818180007,100.61040490631,-65.0339501432301));
#4466=CARTESIAN_POINT('Ctrl Pts',(-72.1150952101049,100.729412390806,-65.2187571487129));
#4467=CARTESIAN_POINT('Ctrl Pts',(-72.3430447123212,101.056823805361,-65.6539018412633));
#4468=CARTESIAN_POINT('Ctrl Pts',(-72.4334348797441,101.308592332847,-65.9279687653144));
#4469=CARTESIAN_POINT('Ctrl Pts',(-72.4840863228325,101.877200205893,-66.4124326626861));
#4470=CARTESIAN_POINT('Ctrl Pts',(-72.4446107771567,102.194506798833,-66.622253399413));
#4471=CARTESIAN_POINT('Ctrl Pts',(-72.2682341952258,102.805493201172,-66.9277466005826));
#4472=CARTESIAN_POINT('Ctrl Pts',(-72.1199499904937,103.138605462879,-67.0431352911788));
#4473=CARTESIAN_POINT('Ctrl Pts',(-71.7245260357815,103.764324604205,-67.1558349009925));
#4474=CARTESIAN_POINT('Ctrl Pts',(-71.4770784393067,104.056618970366,-67.1537994237656));
#4475=CARTESIAN_POINT('Ctrl Pts',(-70.9566767310373,104.524338207794,-67.0632582459091));
#4476=CARTESIAN_POINT('Ctrl Pts',(-70.6485568502061,104.731264722069,-66.968723702923));
#4477=CARTESIAN_POINT('Ctrl Pts',(-70.0050429436934,105.008060588788,-66.7042879633689));
#4478=CARTESIAN_POINT('Ctrl Pts',(-69.6691881895505,105.077430701576,-66.5349861672338));
#4479=CARTESIAN_POINT('Ctrl Pts',(-69.3636718196512,105.077430701576,-66.3585962088306));
#4480=CARTESIAN_POINT('Ctrl Pts',(-69.0581554497519,105.077430701576,-66.1822062504275));
#4481=CARTESIAN_POINT('Ctrl Pts',(-68.7436084163211,105.008060588788,-65.9759983994254));
#4482=CARTESIAN_POINT('Ctrl Pts',(-68.3783111846766,104.824474558597,-65.694061281418));
#4483=CARTESIAN_POINT('Ctrl Pts',(-68.292374214007,104.772275635186,-65.6239319133934));
#4484=CARTESIAN_POINT('Ctrl Pts',(-68.2116924394265,104.714077983567,-65.5538830246511));
#4485=CARTESIAN_POINT('',(-112.569378637745,121.956851469395,-75.7699408736866));
#4486=CARTESIAN_POINT('',(-105.161274966764,121.956851469395,-73.9369105957041));
#4487=CARTESIAN_POINT('Ctrl Pts',(-112.569378637745,121.956851469395,-75.7699408736867));
#4488=CARTESIAN_POINT('Ctrl Pts',(-112.569272008943,121.95672834506,-75.7681386924676));
#4489=CARTESIAN_POINT('Ctrl Pts',(-112.569163342679,121.956605035935,-75.7663364623398));
#4490=CARTESIAN_POINT('Ctrl Pts',(-112.545386428826,121.930081208774,-75.3792452325324));
#4491=CARTESIAN_POINT('Ctrl Pts',(-112.425619842949,121.895265649918,-74.9910716591131));
#4492=CARTESIAN_POINT('Ctrl Pts',(-112.050450493293,121.820378366244,-74.1810533701236));
#4493=CARTESIAN_POINT('Ctrl Pts',(-111.722843184654,121.775514411454,-73.719515362228));
#4494=CARTESIAN_POINT('Ctrl Pts',(-110.943904850608,121.712442638456,-72.9082742376171));
#4495=CARTESIAN_POINT('Ctrl Pts',(-110.491771010159,121.694880858045,-72.5592922284894));
#4496=CARTESIAN_POINT('Ctrl Pts',(-110.03845359778,121.694880858045,-72.2975692984242));
#4497=CARTESIAN_POINT('Ctrl Pts',(-109.648809084286,121.694880858045,-72.07260793367));
#4498=CARTESIAN_POINT('Ctrl Pts',(-109.196813666427,121.708045140711,-71.8773439414328));
#4499=CARTESIAN_POINT('Ctrl Pts',(-108.262263007713,121.76340957246,-71.6499783847423));
#4500=CARTESIAN_POINT('Ctrl Pts',(-107.779465090809,121.805444228819,-71.6188351088017));
#4501=CARTESIAN_POINT('Ctrl Pts',(-106.970686338396,121.883764743458,-71.7387661915901));
#4502=CARTESIAN_POINT('Ctrl Pts',(-106.589756165829,121.923740934709,-71.8676756890549));
#4503=CARTESIAN_POINT('Ctrl Pts',(-105.93403329749,121.982452032228,-72.2850075992705));
#4504=CARTESIAN_POINT('Ctrl Pts',(-105.659130074434,121.999999999998,-72.5734224782579));
#4505=CARTESIAN_POINT('Ctrl Pts',(-105.295732554092,121.999999999998,-73.2028454468363));
#4506=CARTESIAN_POINT('Ctrl Pts',(-105.184827334639,121.984047401261,-73.5660373895111));
#4507=CARTESIAN_POINT('Ctrl Pts',(-105.161274966764,121.956851469395,-73.936910595704));
#4508=CARTESIAN_POINT('Ctrl Pts',(-105.161274966764,121.956851469395,-73.936910595704));
#4509=CARTESIAN_POINT('Ctrl Pts',(-105.160208558995,121.955620087771,-73.9537030502982));
#4510=CARTESIAN_POINT('Ctrl Pts',(-105.159312222542,121.954368073319,-73.9705108670905));
#4511=CARTESIAN_POINT('Ctrl Pts',(-105.141806095166,121.923740934709,-74.3755987782653));
#4512=CARTESIAN_POINT('Ctrl Pts',(-105.220632281856,121.883764743458,-74.7699487335092));
#4513=CARTESIAN_POINT('Ctrl Pts',(-105.521158293664,121.805444228818,-75.5303372205339));
#4514=CARTESIAN_POINT('Ctrl Pts',(-105.789528120238,121.763409572459,-75.9328808434969));
#4515=CARTESIAN_POINT('Ctrl Pts',(-106.453707797634,121.708045140711,-76.628542676721));
#4516=CARTESIAN_POINT('Ctrl Pts',(-106.848809084286,121.694880858045,-76.9223501948628));
#4517=CARTESIAN_POINT('Ctrl Pts',(-107.691771010159,121.694880858045,-77.4090344896822));
#4518=CARTESIAN_POINT('Ctrl Pts',(-108.220065215752,121.712442638456,-77.6261028768581));
#4519=CARTESIAN_POINT('Ctrl Pts',(-109.312089805283,121.775514411454,-77.895062699818));
#4520=CARTESIAN_POINT('Ctrl Pts',(-109.875597099252,121.820378366244,-77.948009947617));
#4521=CARTESIAN_POINT('Ctrl Pts',(-110.764678189875,121.895265649918,-77.8679069906454));
#4522=CARTESIAN_POINT('Ctrl Pts',(-111.160729658472,121.930081208774,-77.7775411098295));
#4523=CARTESIAN_POINT('Ctrl Pts',(-111.678984353092,121.96968170959,-77.5193177005707));
#4524=CARTESIAN_POINT('Ctrl Pts',(-111.839559773292,121.980744602752,-77.4130886523666));
#4525=CARTESIAN_POINT('Ctrl Pts',(-112.11953636853,121.995916933756,-77.161529052004));
#4526=CARTESIAN_POINT('Ctrl Pts',(-112.238887146792,121.999999999998,-77.016140826053));
#4527=CARTESIAN_POINT('Ctrl Pts',(-112.425073184787,121.999999999998,-76.693657148586));
#4528=CARTESIAN_POINT('Ctrl Pts',(-112.491307692741,121.995916933756,-76.5176022296746));
#4529=CARTESIAN_POINT('Ctrl Pts',(-112.568812151847,121.980815574618,-76.1510781390455));
#4530=CARTESIAN_POINT('Ctrl Pts',(-112.580669535468,121.969889075075,-75.9607734026514));
#4531=CARTESIAN_POINT('Ctrl Pts',(-112.569378637745,121.956851469395,-75.7699408736867));
#4532=CARTESIAN_POINT('',(-101.043673435707,121.93955176967,-68.8916782754278));
#4533=CARTESIAN_POINT('',(-94.7826830987082,121.939551769669,-68.1687213841338));
#4534=CARTESIAN_POINT('Ctrl Pts',(-101.043673435707,121.93955176967,-68.8916782754277));
#4535=CARTESIAN_POINT('Ctrl Pts',(-101.030778440127,121.913761778509,-68.5765055229452));
#4536=CARTESIAN_POINT('Ctrl Pts',(-100.960164861362,121.882510881795,-68.2634583404383));
#4537=CARTESIAN_POINT('Ctrl Pts',(-100.712810634339,121.813417983957,-67.5935677254039));
#4538=CARTESIAN_POINT('Ctrl Pts',(-100.483220636953,121.771343589081,-67.2056047409378));
#4539=CARTESIAN_POINT('Ctrl Pts',(-99.9029587467504,121.711697111731,-66.5303819021385));
#4540=CARTESIAN_POINT('Ctrl Pts',(-99.5520623213409,121.694880858045,-66.2432484721442));
#4541=CARTESIAN_POINT('Ctrl Pts',(-99.1908428113955,121.694880858045,-66.0346982908408));
#4542=CARTESIAN_POINT('Ctrl Pts',(-98.8578333531796,121.694880858045,-65.8424351904971));
#4543=CARTESIAN_POINT('Ctrl Pts',(-98.4675142149001,121.709425126322,-65.6899158622252));
#4544=CARTESIAN_POINT('Ctrl Pts',(-97.6636618634519,121.766292452039,-65.5478256106297));
#4545=CARTESIAN_POINT('Ctrl Pts',(-97.2499629860219,121.808024204338,-65.5589567845263));
#4546=CARTESIAN_POINT('Ctrl Pts',(-96.532228635356,121.885750778307,-65.7270017969835));
#4547=CARTESIAN_POINT('Ctrl Pts',(-96.1806212553106,121.926229231586,-65.8836810953591));
#4548=CARTESIAN_POINT('Ctrl Pts',(-95.5755231979279,121.983802794611,-66.3313873276683));
#4549=CARTESIAN_POINT('Ctrl Pts',(-95.3217546974658,121.999999999998,-66.6221537056877));
#4550=CARTESIAN_POINT('Ctrl Pts',(-94.9650500672789,121.999999999998,-67.2399842484664));
#4551=CARTESIAN_POINT('Ctrl Pts',(-94.8401232475787,121.983802794611,-67.6051374055565));
#4552=CARTESIAN_POINT('Ctrl Pts',(-94.7903548426391,121.950162492739,-68.0421265757317));
#4553=CARTESIAN_POINT('Ctrl Pts',(-94.7854013049624,121.944988182178,-68.1054231196404));
#4554=CARTESIAN_POINT('Ctrl Pts',(-94.7826830987084,121.93955176967,-68.168721384132));
#4555=CARTESIAN_POINT('Ctrl Pts',(-94.7826830987083,121.93955176967,-68.168721384132));
#4556=CARTESIAN_POINT('Ctrl Pts',(-94.7692793143766,121.912744201006,-68.4808523287743));
#4557=CARTESIAN_POINT('Ctrl Pts',(-94.8123721828179,121.87944427626,-68.7931115535356));
#4558=CARTESIAN_POINT('Ctrl Pts',(-95.0083986686057,121.808024204338,-69.4414600707244));
#4559=CARTESIAN_POINT('Ctrl Pts',(-95.2056082279524,121.766292452039,-69.8052993950442));
#4560=CARTESIAN_POINT('Ctrl Pts',(-95.7305881711883,121.709425126322,-70.4304108264924));
#4561=CARTESIAN_POINT('Ctrl Pts',(-96.0578333531797,121.694880858045,-70.6921774516898));
#4562=CARTESIAN_POINT('Ctrl Pts',(-96.7520623213409,121.694880858045,-71.0929907333369));
#4563=CARTESIAN_POINT('Ctrl Pts',(-97.1761753786965,121.711697111731,-71.2533092368416));
#4564=CARTESIAN_POINT('Ctrl Pts',(-98.0510664554135,121.771343589081,-71.4182193552053));
#4565=CARTESIAN_POINT('Ctrl Pts',(-98.5018472543822,121.813417983957,-71.4230686331636));
#4566=CARTESIAN_POINT('Ctrl Pts',(-99.2682419576485,121.888653805311,-71.2916044625037));
#4567=CARTESIAN_POINT('Ctrl Pts',(-99.6421808158843,121.927100882661,-71.163309142685));
#4568=CARTESIAN_POINT('Ctrl Pts',(-100.289083992022,121.983258351228,-70.7579195346131));
#4569=CARTESIAN_POINT('Ctrl Pts',(-100.561342752554,121.999999999998,-70.4795670133904));
#4570=CARTESIAN_POINT('Ctrl Pts',(-100.92546201219,121.999999999998,-69.8488939556873));
#4571=CARTESIAN_POINT('Ctrl Pts',(-101.03039298651,121.983258351228,-69.4739346920516));
#4572=CARTESIAN_POINT('Ctrl Pts',(-101.046625787479,121.950260836241,-69.0256457187578));
#4573=CARTESIAN_POINT('Ctrl Pts',(-101.046412113711,121.945029125677,-68.9586156139657));
#4574=CARTESIAN_POINT('Ctrl Pts',(-101.043673435707,121.93955176967,-68.8916782754277));
#4575=CARTESIAN_POINT('',(-89.6457108608091,121.928269354306,-62.1822365876521));
#4576=CARTESIAN_POINT('',(-83.8969144629603,121.928269354306,-62.0126448588956));
#4577=CARTESIAN_POINT('Ctrl Pts',(-89.6457108608091,121.928269354306,-62.1822365876521));
#4578=CARTESIAN_POINT('Ctrl Pts',(-89.640048215299,121.903866743648,-61.9118469440624));
#4579=CARTESIAN_POINT('Ctrl Pts',(-89.5938110699338,121.875525701933,-61.6447310127997));
#4580=CARTESIAN_POINT('Ctrl Pts',(-89.4114212651875,121.810267922929,-61.0498367272997));
#4581=CARTESIAN_POINT('Ctrl Pts',(-89.2283577823594,121.76941928365,-60.6962570673076));
#4582=CARTESIAN_POINT('Ctrl Pts',(-88.7408793475757,121.711304602249,-60.0841026261431));
#4583=CARTESIAN_POINT('Ctrl Pts',(-88.4363138250625,121.694880858045,-59.8255680855737));
#4584=CARTESIAN_POINT('Ctrl Pts',(-88.11715467285,121.694880858045,-59.6413014631295));
#4585=CARTESIAN_POINT('Ctrl Pts',(-87.8077521236662,121.694880858045,-59.4626678180703));
#4586=CARTESIAN_POINT('Ctrl Pts',(-87.4431698769551,121.710493799957,-59.3305852473804));
#4587=CARTESIAN_POINT('Ctrl Pts',(-86.6945172380366,121.768237475725,-59.2263000150256));
#4588=CARTESIAN_POINT('Ctrl Pts',(-86.3103592215609,121.809531015002,-59.2542646021946));
#4589=CARTESIAN_POINT('Ctrl Pts',(-85.6299700128694,121.886577617489,-59.4387756069027));
#4590=CARTESIAN_POINT('Ctrl Pts',(-85.2887695763051,121.927161354661,-59.6051048904537));
#4591=CARTESIAN_POINT('Ctrl Pts',(-84.7006180249038,121.984260557561,-60.0622377416933));
#4592=CARTESIAN_POINT('Ctrl Pts',(-84.4534935750556,121.999999999998,-60.35291487129));
#4593=CARTESIAN_POINT('Ctrl Pts',(-84.1015994130934,121.999999999998,-60.9624134386954));
#4594=CARTESIAN_POINT('Ctrl Pts',(-83.9734278594876,121.98426055756,-61.3217680549585));
#4595=CARTESIAN_POINT('Ctrl Pts',(-83.9077720873625,121.947439165029,-61.7976287162892));
#4596=CARTESIAN_POINT('Ctrl Pts',(-83.8992173832946,121.938193561674,-61.9053402793198));
#4597=CARTESIAN_POINT('Ctrl Pts',(-83.8969144629603,121.928269354306,-62.0126448588956));
#4598=CARTESIAN_POINT('Ctrl Pts',(-83.8969144629603,121.928269354306,-62.0126448588956));
#4599=CARTESIAN_POINT('Ctrl Pts',(-83.8912689889189,121.903940742393,-62.2756957380355));
#4600=CARTESIAN_POINT('Ctrl Pts',(-83.9241062924374,121.875500673982,-62.5363189359234));
#4601=CARTESIAN_POINT('Ctrl Pts',(-84.0785731934348,121.809531015002,-63.1198313945313));
#4602=CARTESIAN_POINT('Ctrl Pts',(-84.246434158778,121.768237475725,-63.4665042894511));
#4603=CARTESIAN_POINT('Ctrl Pts',(-84.7110741386961,121.710493799957,-64.0627138771875));
#4604=CARTESIAN_POINT('Ctrl Pts',(-85.0077521236662,121.694880858045,-64.3124100792631));
#4605=CARTESIAN_POINT('Ctrl Pts',(-85.6363138250625,121.694880858045,-64.6753103467665));
#4606=CARTESIAN_POINT('Ctrl Pts',(-86.012494066208,121.711304602249,-64.8098045560952));
#4607=CARTESIAN_POINT('Ctrl Pts',(-86.7863745806878,121.76941928365,-64.9258960438327));
#4608=CARTESIAN_POINT('Ctrl Pts',(-87.1841152899164,121.810267922929,-64.907643840471));
#4609=CARTESIAN_POINT('Ctrl Pts',(-87.8886874328802,121.886091946244,-64.7455648365782));
#4610=CARTESIAN_POINT('Ctrl Pts',(-88.245336954858,121.9263037894,-64.5935914546221));
#4611=CARTESIAN_POINT('Ctrl Pts',(-88.8607180558249,121.983695909948,-64.1544777755007));
#4612=CARTESIAN_POINT('Ctrl Pts',(-89.1191660952628,121.999999999998,-63.866826235406));
#4613=CARTESIAN_POINT('Ctrl Pts',(-89.4775721811683,121.999999999998,-63.2460486848757));
#4614=CARTESIAN_POINT('Ctrl Pts',(-89.5974617026091,121.983695909948,-62.8784003471169));
#4615=CARTESIAN_POINT('Ctrl Pts',(-89.6440171485706,121.946889139357,-62.3958111209995));
#4616=CARTESIAN_POINT('Ctrl Pts',(-89.6479419658163,121.937884080627,-62.2887711900116));
#4617=CARTESIAN_POINT('Ctrl Pts',(-89.6457108608091,121.928269354306,-62.1822365876521));
#4618=CARTESIAN_POINT('',(-75.5607164801933,121.77184403287,-52.8249999999979));
#4619=CARTESIAN_POINT('',(-75.5607164801932,121.77184403287,-58.4249999999981));
#4620=CARTESIAN_POINT('Ctrl Pts',(-75.5607164801933,121.77184403287,-52.8249999999979));
#4621=CARTESIAN_POINT('Ctrl Pts',(-75.31087199813,121.795561855846,-52.8249999999979));
#4622=CARTESIAN_POINT('Ctrl Pts',(-75.0641712044988,121.822609441991,-52.8592756004775));
#4623=CARTESIAN_POINT('Ctrl Pts',(-74.4972946958141,121.886557224277,-53.0111697031877));
#4624=CARTESIAN_POINT('Ctrl Pts',(-74.1537701819123,121.927083062952,-53.1755443283788));
#4625=CARTESIAN_POINT('Ctrl Pts',(-73.561230066802,121.984194331231,-53.6296591429951));
#4626=CARTESIAN_POINT('Ctrl Pts',(-73.3122219315277,121.999999999998,-53.9195067988283));
#4627=CARTESIAN_POINT('Ctrl Pts',(-72.9594687676658,121.999999999998,-54.5304932011677));
#4628=CARTESIAN_POINT('Ctrl Pts',(-72.8329574021241,121.984194331231,-54.8910643999808));
#4629=CARTESIAN_POINT('Ctrl Pts',(-72.7359524939867,121.927083062952,-55.6312765997358));
#4630=CARTESIAN_POINT('Ctrl Pts',(-72.7653621497846,121.886557224277,-56.010964868193));
#4631=CARTESIAN_POINT('Ctrl Pts',(-72.9468930668116,121.810132271938,-56.6884474736823));
#4632=CARTESIAN_POINT('Ctrl Pts',(-73.1112681701126,121.769187929666,-57.0319552746733));
#4633=CARTESIAN_POINT('Ctrl Pts',(-73.5653642866542,121.711112887006,-57.6244722503148));
#4634=CARTESIAN_POINT('Ctrl Pts',(-73.855200110294,121.694880858045,-57.8734811721914));
#4635=CARTESIAN_POINT('Ctrl Pts',(-74.4662328500925,121.694880858045,-58.2262610889977));
#4636=CARTESIAN_POINT('Ctrl Pts',(-74.8267988140265,121.711112887006,-58.3527618142583));
#4637=CARTESIAN_POINT('Ctrl Pts',(-75.3177281966151,121.749631404864,-58.4170976637661));
#4638=CARTESIAN_POINT('Ctrl Pts',(-75.4395919608409,121.760345640413,-58.4249999999981));
#4639=CARTESIAN_POINT('Ctrl Pts',(-75.560716480193,121.77184403287,-58.4249999999981));
#4640=CARTESIAN_POINT('Ctrl Pts',(-75.560716480193,121.77184403287,-58.4249999999981));
#4641=CARTESIAN_POINT('Ctrl Pts',(-75.8105609622564,121.795561855846,-58.4249999999981));
#4642=CARTESIAN_POINT('Ctrl Pts',(-76.0572617558877,121.822609441991,-58.3907243995186));
#4643=CARTESIAN_POINT('Ctrl Pts',(-76.6241382645725,121.886557224277,-58.2388302968083));
#4644=CARTESIAN_POINT('Ctrl Pts',(-76.9676627784743,121.927083062952,-58.0744556716172));
#4645=CARTESIAN_POINT('Ctrl Pts',(-77.5602028935846,121.984194331231,-57.620340857001));
#4646=CARTESIAN_POINT('Ctrl Pts',(-77.8092110288589,121.999999999998,-57.3304932011678));
#4647=CARTESIAN_POINT('Ctrl Pts',(-78.1619641927208,121.999999999998,-56.7195067988283));
#4648=CARTESIAN_POINT('Ctrl Pts',(-78.2884755582626,121.984194331231,-56.3589356000152));
#4649=CARTESIAN_POINT('Ctrl Pts',(-78.3854804663999,121.927083062952,-55.6187234002602));
#4650=CARTESIAN_POINT('Ctrl Pts',(-78.356070810602,121.886557224277,-55.239035131803));
#4651=CARTESIAN_POINT('Ctrl Pts',(-78.174539893575,121.810132271938,-54.5615525263137));
#4652=CARTESIAN_POINT('Ctrl Pts',(-78.010164790274,121.769187929666,-54.2180447253227));
#4653=CARTESIAN_POINT('Ctrl Pts',(-77.5560686737324,121.711112887006,-53.6255277496812));
#4654=CARTESIAN_POINT('Ctrl Pts',(-77.2662328500926,121.694880858045,-53.3765188278046));
#4655=CARTESIAN_POINT('Ctrl Pts',(-76.9607164801934,121.694880858045,-53.2001288694015));
#4656=CARTESIAN_POINT('Ctrl Pts',(-76.6552001102941,121.694880858045,-53.0237389109983));
#4657=CARTESIAN_POINT('Ctrl Pts',(-76.2946341463601,121.711112887006,-52.8972381857377));
#4658=CARTESIAN_POINT('Ctrl Pts',(-75.8037047637714,121.749631404864,-52.8329023362299));
#4659=CARTESIAN_POINT('Ctrl Pts',(-75.6818409995455,121.760345640413,-52.8249999999979));
#4660=CARTESIAN_POINT('Ctrl Pts',(-75.5607164801933,121.77184403287,-52.8249999999979));
#4661=CARTESIAN_POINT('Origin',(-115.614391405224,109.,-78.7499999999976));
#4662=CARTESIAN_POINT('Origin',(-111.692877174869,125.221825406948,-76.4859127034721));
#4663=CARTESIAN_POINT('',(-109.047125863805,127.513113254426,-76.4859127034721));
#4664=CARTESIAN_POINT('Origin',(-111.692877174869,125.221825406948,-76.4859127034721));
#4665=CARTESIAN_POINT('',(-109.576276126018,127.054855684931,-76.4859127034722));
#4666=CARTESIAN_POINT('Origin',(-111.692877174869,125.221825406948,-76.4859127034722));
#4667=CARTESIAN_POINT('Origin',(-111.692877174869,125.221825406948,-76.4859127034721));
#4668=CARTESIAN_POINT('',(-109.047125863805,127.513113254426,-76.4859127034721));
#4669=CARTESIAN_POINT('Origin',(-75.5607164801933,112.,-55.624999999998));
#4670=CARTESIAN_POINT('',(-75.5607164801933,112.,-58.4249999999981));
#4671=CARTESIAN_POINT('Origin',(-84.3932587967998,111.68028146752,-60.7244706841197));
#4672=CARTESIAN_POINT('',(-81.6657313432502,112.313206415782,-60.7244706841197));
#4673=CARTESIAN_POINT('Origin',(-93.3501356426365,112.813466520527,-65.8957259421618));
#4674=CARTESIAN_POINT('',(-90.8457395078369,114.065664587927,-65.8957259421618));
#4675=CARTESIAN_POINT('Origin',(-103.119663075128,115.322330470337,-71.5361652351663));
#4676=CARTESIAN_POINT('',(-101.003062026277,117.155360748319,-71.5361652351663));
#4677=CARTESIAN_POINT('Origin',(-84.2209705180366,98.999999999999,-40.6249999999996));
#4678=CARTESIAN_POINT('',(-86.8190467293899,101.999999999999,-40.1249999999996));
#4679=CARTESIAN_POINT('Origin',(-84.2209705180366,98.999999999999,-40.6249999999996));
#4680=CARTESIAN_POINT('',(-86.4942872029708,101.624999999999,-40.1874999999995));
#4681=CARTESIAN_POINT('Origin',(-84.2209705180366,98.999999999999,-40.6249999999996));
#4682=CARTESIAN_POINT('Origin',(-26.1968246264604,166.000512499998,-141.125768750001));
#4683=CARTESIAN_POINT('',(-28.7949008378137,169.000512499998,-140.625768750001));
#4684=CARTESIAN_POINT('',(-80.5957703324788,98.5672184524782,-46.904030908994));
#4685=CARTESIAN_POINT('',(-80.5957703324788,98.567218452478,-46.9040309089941));
#4686=CARTESIAN_POINT('',(-82.595770332479,105.495421682753,-43.4399292938557));
#4687=CARTESIAN_POINT('Ctrl Pts',(-80.5957703324787,98.5672184524781,-46.9040309089941));
#4688=CARTESIAN_POINT('Ctrl Pts',(-80.1583076046396,98.5672184524781,-46.6514616853158));
#4689=CARTESIAN_POINT('Ctrl Pts',(-79.731847375509,98.6399471087077,-46.316319579711));
#4690=CARTESIAN_POINT('Ctrl Pts',(-79.0280064685973,98.9402745490956,-45.5660699284182));
#4691=CARTESIAN_POINT('Ctrl Pts',(-78.7496249554672,99.168633673537,-45.1522067177974));
#4692=CARTESIAN_POINT('Ctrl Pts',(-78.3748022679429,99.7108672272503,-44.3867423304201));
#4693=CARTESIAN_POINT('Ctrl Pts',(-78.2527827584179,100.061688880156,-43.983215927173));
#4694=CARTESIAN_POINT('Ctrl Pts',(-78.1901153330479,100.862134488935,-43.2736771449321));
#4695=CARTESIAN_POINT('Ctrl Pts',(-78.2490409596484,101.312629171298,-42.9686854143502));
#4696=CARTESIAN_POINT('Ctrl Pts',(-78.5015571253347,102.1873708287,-42.531314585649));
#4697=CARTESIAN_POINT('Ctrl Pts',(-78.7110997683144,102.666877512603,-42.3713056330979));
#4698=CARTESIAN_POINT('Ctrl Pts',(-79.2661565338858,103.572118612493,-42.2280010610046));
#4699=CARTESIAN_POINT('Ctrl Pts',(-79.6121998656049,103.997338243878,-42.2435068221059));
#4700=CARTESIAN_POINT('Ctrl Pts',(-80.340691634629,104.680250326612,-42.3963983912593));
#4701=CARTESIAN_POINT('Ctrl Pts',(-80.7727618736163,104.984284565641,-42.5440649201448));
#4702=CARTESIAN_POINT('Ctrl Pts',(-81.6811020778789,105.3923634715,-42.9401113983139));
#4703=CARTESIAN_POINT('Ctrl Pts',(-82.15830760464,105.495421682753,-43.1873600701774));
#4704=CARTESIAN_POINT('Ctrl Pts',(-82.595770332479,105.495421682753,-43.4399292938557));
#4705=CARTESIAN_POINT('',(-82.595770332479,105.495421682753,-43.4399292938557));
#4706=CARTESIAN_POINT('Origin',(-66.9004624423481,99.0000000000011,-70.6249999999998));
#4707=CARTESIAN_POINT('',(-69.4985386537014,96.000000000001,-70.1249999999998));
#4708=CARTESIAN_POINT('Origin',(-66.9004624423481,99.0000000000011,-70.6249999999998));
#4709=CARTESIAN_POINT('',(-69.1737791272823,96.375000000001,-70.1874999999998));
#4710=CARTESIAN_POINT('Origin',(-66.9004624423481,99.0000000000011,-70.6249999999998));
#4711=CARTESIAN_POINT('Origin',(-124.924608333924,166.000512500002,29.8757687500004));
#4712=CARTESIAN_POINT('',(-127.522684545277,163.000512500001,30.3757687500005));
#4713=CARTESIAN_POINT('',(-68.5256626279059,105.495421682756,-67.8100707061432));
#4714=CARTESIAN_POINT('',(-68.5256626279059,105.495421682756,-67.8100707061433));
#4715=CARTESIAN_POINT('',(-70.5256626279056,98.5672184524799,-64.3459690910059));
#4716=CARTESIAN_POINT('Ctrl Pts',(-68.5256626279059,105.495421682756,-67.8100707061432));
#4717=CARTESIAN_POINT('Ctrl Pts',(-68.0881999000668,105.495421682756,-67.5575014824649));
#4718=CARTESIAN_POINT('Ctrl Pts',(-67.6354735058005,105.392363471503,-67.2678537093952));
#4719=CARTESIAN_POINT('Ctrl Pts',(-66.8383170924954,104.984284565643,-66.6792312563097));
#4720=CARTESIAN_POINT('Ctrl Pts',(-66.4943990076982,104.680250326615,-66.3788807175702));
#4721=CARTESIAN_POINT('Ctrl Pts',(-65.9977451402748,103.99733824388,-65.8244341237244));
#4722=CARTESIAN_POINT('Ctrl Pts',(-65.8112950913965,103.572118612495,-65.5325046881962));
#4723=CARTESIAN_POINT('Ctrl Pts',(-65.657872108522,102.666877512605,-64.9801591426223));
#4724=CARTESIAN_POINT('Ctrl Pts',(-65.6916726047743,102.187370828702,-64.7186854143503));
#4725=CARTESIAN_POINT('Ctrl Pts',(-65.9441887704605,101.3126291713,-64.2813145856493));
#4726=CARTESIAN_POINT('Ctrl Pts',(-66.1788565437883,100.862134488937,-64.0777876307885));
#4727=CARTESIAN_POINT('Ctrl Pts',(-66.8246688668641,100.061688880158,-63.7772898220283));
#4728=CARTESIAN_POINT('Ctrl Pts',(-67.2351427379364,99.7108672272523,-63.6811986154108));
#4729=CARTESIAN_POINT('Ctrl Pts',(-68.0854656868595,99.1686336735389,-63.623072391033));
#4730=CARTESIAN_POINT('Ctrl Pts',(-68.5830724975138,98.9402745490975,-63.6572262480373));
#4731=CARTESIAN_POINT('Ctrl Pts',(-69.5847282081697,98.6399471087095,-63.8916455279991));
#4732=CARTESIAN_POINT('Ctrl Pts',(-70.0881999000665,98.5672184524799,-64.0933998673275));
#4733=CARTESIAN_POINT('Ctrl Pts',(-70.5256626279056,98.5672184524799,-64.3459690910059));
#4734=CARTESIAN_POINT('',(-70.5256626279056,98.5672184524799,-64.3459690910059));
#4735=CARTESIAN_POINT('Origin',(-96.4746890553668,99.4494897427822,-48.5986671816671));
#4736=CARTESIAN_POINT('',(-94.430917460329,100.684620539947,-45.3897032396429));
#4737=CARTESIAN_POINT('Origin',(-96.4746890553668,99.4494897427822,-48.5986671816671));
#4738=CARTESIAN_POINT('',(-94.6863889097089,100.530229190302,-45.7908237323958));
#4739=CARTESIAN_POINT('Origin',(-96.4746890553669,99.4494897427822,-48.598667181667));
#4740=CARTESIAN_POINT('Origin',(41.8109368646032,203.413715679656,-176.687875705469));
#4741=CARTESIAN_POINT('',(43.8547084596409,204.648846476821,-173.478911763445));
#4742=CARTESIAN_POINT('Origin',(-79.9327200516597,99.449489742784,-77.250197953318));
#4743=CARTESIAN_POINT('',(-77.1059069082159,97.3101804481012,-75.3975017575705));
#4744=CARTESIAN_POINT('Origin',(-79.9327200516597,99.449489742784,-77.250197953318));
#4745=CARTESIAN_POINT('',(-77.4592585511463,97.5775941099365,-75.629088782039));
#4746=CARTESIAN_POINT('Origin',(-79.9327200516597,99.4494897427839,-77.250197953318));
#4747=CARTESIAN_POINT('Origin',(-121.718415623925,203.413715679661,106.553271333508));
#4748=CARTESIAN_POINT('',(-118.891602480482,201.274406384978,108.405967529256));
#4749=CARTESIAN_POINT('Origin',(-108.737631016432,99.7320508075681,-56.2438021535162));
#4750=CARTESIAN_POINT('',(-107.276159708174,100.386816955051,-52.5783713592919));
#4751=CARTESIAN_POINT('Origin',(-108.737631016432,99.7320508075681,-56.2438021535162));
#4752=CARTESIAN_POINT('',(-107.458843621706,100.304971186616,-53.03655020857));
#4753=CARTESIAN_POINT('Origin',(-108.737631016432,99.732050807568,-56.2438021535162));
#4754=CARTESIAN_POINT('Origin',(125.171333134686,225.083486900949,-171.899270921774));
#4755=CARTESIAN_POINT('',(126.632804442944,225.738253048432,-168.23384012755));
#4756=CARTESIAN_POINT('Origin',(-92.6850721331748,99.7320508075696,-84.0476497308099));
#4757=CARTESIAN_POINT('',(-89.6744074864335,97.2884302780867,-83.0655005095853));
#4758=CARTESIAN_POINT('Origin',(-92.6850721331748,99.7320508075696,-84.0476497308099));
#4759=CARTESIAN_POINT('',(-90.0507405672762,97.5938828442721,-83.1882691622385));
#4760=CARTESIAN_POINT('Origin',(-92.6850721331748,99.7320508075696,-84.0476497308099));
#4761=CARTESIAN_POINT('Origin',(-75.8911640975186,225.083486900956,176.351189781088));
#4762=CARTESIAN_POINT('',(-72.8804994507773,222.639866371473,177.333339002313));
#4763=CARTESIAN_POINT('Origin',(-121.472809584586,99.8284271247455,-63.7892135623721));
#4764=CARTESIAN_POINT('',(-120.716880638568,99.8284271247455,-59.8612915381242));
#4765=CARTESIAN_POINT('Origin',(-121.472809584586,99.8284271247455,-63.7892135623721));
#4766=CARTESIAN_POINT('',(-120.81137175682,99.8284271247455,-60.3522817911552));
#4767=CARTESIAN_POINT('Origin',(-121.472809584586,99.8284271247455,-63.7892135623721));
#4768=CARTESIAN_POINT('Origin',(201.051502502506,223.968092727195,-125.859046363603));
#4769=CARTESIAN_POINT('',(201.807431448525,223.968092727195,-121.931124339356));
#4770=CARTESIAN_POINT('Origin',(-105.587179379326,99.8284271247468,-91.303932188134));
#4771=CARTESIAN_POINT('',(-102.563463595252,97.2098124419149,-91.303932188134));
#4772=CARTESIAN_POINT('Origin',(-105.587179379326,99.8284271247468,-91.303932188134));
#4773=CARTESIAN_POINT('',(-102.941428068262,97.5371392772689,-91.303932188134));
#4774=CARTESIAN_POINT('Origin',(-105.587179379326,99.8284271247468,-91.303932188134));
#4775=CARTESIAN_POINT('Origin',(1.92092464970915,223.968092727204,219.045231817999));
#4776=CARTESIAN_POINT('',(4.94464043378298,221.349478044372,219.045231817999));
#4777=CARTESIAN_POINT('Origin',(-74.2616783745156,107.500000000001,-57.8749999999998));
#4778=CARTESIAN_POINT('',(-70.018153895972,98.4000000000012,-68.0249999999999));
#4779=CARTESIAN_POINT('',(-76.080331722463,105.400000000001,-57.5249999999998));
#4780=CARTESIAN_POINT('Origin',(-68.1995005480246,100.500000000001,-68.3749999999999));
#4781=CARTESIAN_POINT('Origin',(-76.8597545858689,107.499999999999,-53.3749999999998));
#4782=CARTESIAN_POINT('',(-84.7405857603073,102.599999999999,-42.5249999999996));
#4783=CARTESIAN_POINT('',(-78.6784079338163,109.599999999999,-53.0249999999997));
#4784=CARTESIAN_POINT('Origin',(-82.9219324123599,100.499999999999,-42.8749999999997));
#4785=CARTESIAN_POINT('Origin',(-83.2326628767165,107.659859266241,-62.734681784761));
#4786=CARTESIAN_POINT('',(-78.5362937027295,99.4008619759398,-73.3917489394908));
#4787=CARTESIAN_POINT('',(-81.2538936763059,106.162342759963,-61.4377944477378));
#4788=CARTESIAN_POINT('Origin',(-80.5150629031402,100.898378482218,-74.6886362765139));
#4789=CARTESIAN_POINT('Origin',(-85.5538547168813,107.659859266239,-58.7142595834813));
#4790=CARTESIAN_POINT('',(-93.1168428791077,101.762970040231,-48.1374969637468));
#4791=CARTESIAN_POINT('',(-84.1232146003549,108.524450824255,-56.4679848240644));
#4792=CARTESIAN_POINT('Origin',(-94.5474829956341,100.898378482216,-50.3837717231637));
#4793=CARTESIAN_POINT('Origin',(-91.6988562010068,107.093266739737,-68.7558258325585));
#4794=CARTESIAN_POINT('',(-90.4035687747792,99.3205545426085,-80.661588117438));
#4795=CARTESIAN_POINT('',(-89.5913909482879,105.3827323691,-68.0683213777014));
#4796=CARTESIAN_POINT('Origin',(-92.511034027498,101.031088913246,-81.3490925722951));
#4797=CARTESIAN_POINT('Origin',(-95.0014150842646,107.093266739736,-63.0356260517679));
#4798=CARTESIAN_POINT('',(-105.290562994975,101.489425216483,-54.8765577560743));
#4799=CARTESIAN_POINT('',(-93.9783851684838,107.551603042974,-60.469824495811));
#4800=CARTESIAN_POINT('Origin',(-106.313592910756,101.031088913245,-57.4423593120313));
#4801=CARTESIAN_POINT('Origin',(-100.382013675912,105.838834764833,-76.2779130879201));
#4802=CARTESIAN_POINT('',(-102.552019676931,99.0560570185445,-88.6522817586846));
#4803=CARTESIAN_POINT('',(-98.2654126270599,104.00580448685,-76.2779130879202));
#4804=CARTESIAN_POINT('Origin',(-104.668620725782,100.889087296527,-88.6522817586846));
#4805=CARTESIAN_POINT('Origin',(-105.857312474343,105.838834764831,-66.7944173824152));
#4806=CARTESIAN_POINT('',(-118.187983361742,100.889087296525,-61.5699982312887));
#4807=CARTESIAN_POINT('',(-105.328162212131,105.838834764831,-64.0448719654417));
#4808=CARTESIAN_POINT('Origin',(-118.717133623955,100.889087296525,-64.3195436482622));
#4809=CARTESIAN_POINT('Origin',(-82.9219324123599,100.499999999999,-42.8749999999996));
#4810=CARTESIAN_POINT('',(-85.1952490972941,103.124999999999,-42.4374999999996));
#4811=CARTESIAN_POINT('Origin',(-82.9219324123599,100.499999999999,-42.8749999999996));
#4812=CARTESIAN_POINT('Origin',(-82.9219324123599,100.499999999999,-42.8749999999996));
#4813=CARTESIAN_POINT('',(-85.1952490972941,103.124999999999,-42.4374999999996));
#4814=CARTESIAN_POINT('Origin',(-68.1995005480247,100.500000000001,-68.3749999999998));
#4815=CARTESIAN_POINT('',(-70.4728172329589,97.875000000001,-67.9374999999998));
#4816=CARTESIAN_POINT('Origin',(-68.1995005480247,100.500000000001,-68.3749999999998));
#4817=CARTESIAN_POINT('Origin',(-68.1995005480247,100.500000000001,-68.3749999999998));
#4818=CARTESIAN_POINT('',(-70.4728172329589,97.875000000001,-67.9374999999998));
#4819=CARTESIAN_POINT('Origin',(-94.5474829956341,100.898378482216,-50.3837717231636));
#4820=CARTESIAN_POINT('',(-92.7591828499761,101.979117929735,-47.5759282738925));
#4821=CARTESIAN_POINT('Origin',(-94.5474829956341,100.898378482216,-50.3837717231636));
#4822=CARTESIAN_POINT('Origin',(-94.5474829956341,100.898378482216,-50.3837717231636));
#4823=CARTESIAN_POINT('',(-92.7591828499761,101.979117929735,-47.5759282738925));
#4824=CARTESIAN_POINT('Origin',(-80.5150629031403,100.898378482218,-74.6886362765138));
#4825=CARTESIAN_POINT('',(-78.041601402627,99.0264828493701,-73.0675271052348));
#4826=CARTESIAN_POINT('Origin',(-80.5150629031403,100.898378482218,-74.6886362765138));
#4827=CARTESIAN_POINT('Origin',(-80.5150629031403,100.898378482218,-74.6886362765138));
#4828=CARTESIAN_POINT('',(-78.041601402627,99.0264828493701,-73.0675271052348));
#4829=CARTESIAN_POINT('Origin',(-106.313592910756,101.031088913245,-57.4423593120312));
#4830=CARTESIAN_POINT('',(-105.03480551603,101.604009292292,-54.235107367085));
#4831=CARTESIAN_POINT('Origin',(-106.313592910756,101.031088913245,-57.4423593120312));
#4832=CARTESIAN_POINT('Origin',(-106.313592910756,101.031088913245,-57.4423593120312));
#4833=CARTESIAN_POINT('',(-105.03480551603,101.604009292292,-54.235107367085));
#4834=CARTESIAN_POINT('Origin',(-92.5110340274981,101.031088913246,-81.349092572295));
#4835=CARTESIAN_POINT('',(-89.8767024615995,98.8929209499488,-80.4897120037236));
#4836=CARTESIAN_POINT('Origin',(-92.5110340274981,101.031088913246,-81.349092572295));
#4837=CARTESIAN_POINT('Origin',(-92.5110340274981,101.031088913246,-81.349092572295));
#4838=CARTESIAN_POINT('',(-89.8767024615995,98.8929209499488,-80.4897120037236));
#4839=CARTESIAN_POINT('Origin',(-118.717133623955,100.889087296525,-64.319543648262));
#4840=CARTESIAN_POINT('',(-118.055695796189,100.889087296525,-60.8826118770452));
#4841=CARTESIAN_POINT('Origin',(-118.717133623955,100.889087296525,-64.319543648262));
#4842=CARTESIAN_POINT('Origin',(-118.717133623955,100.889087296525,-64.319543648262));
#4843=CARTESIAN_POINT('',(-118.055695796189,100.889087296525,-60.8826118770452));
#4844=CARTESIAN_POINT('Origin',(-104.668620725782,100.889087296527,-88.6522817586845));
#4845=CARTESIAN_POINT('',(-102.022869414718,98.5977994490487,-88.6522817586845));
#4846=CARTESIAN_POINT('Origin',(-104.668620725782,100.889087296527,-88.6522817586845));
#4847=CARTESIAN_POINT('Origin',(-104.668620725782,100.889087296527,-88.6522817586845));
#4848=CARTESIAN_POINT('',(-102.022869414718,98.5977994490487,-88.6522817586845));
#4849=CARTESIAN_POINT('Origin',(-125.268934230709,90.999,-76.5975199760558));
#4850=CARTESIAN_POINT('',(-122.424179917669,121.863728726179,-74.9551003076436));
#4851=CARTESIAN_POINT('Origin',(-118.577560436093,90.999,-88.1873193607661));
#4852=CARTESIAN_POINT('',(-115.732806123053,121.863728726179,-86.5448996923539));
#4853=CARTESIAN_POINT('Origin',(-115.529994481957,90.999,-74.0824712601139));
#4854=CARTESIAN_POINT('',(-115.529994481957,122.937359864766,-74.0824712601139));
#4855=CARTESIAN_POINT('',(-115.529994481957,122.937359864766,-74.0824712601139));
#4856=CARTESIAN_POINT('',(-115.529994481957,122.937359864766,-74.082471260114));
#4857=CARTESIAN_POINT('Origin',(-111.529994481957,90.999,-81.0106744903897));
#4858=CARTESIAN_POINT('',(-111.529994481957,122.937359864767,-81.0106744903897));
#4859=CARTESIAN_POINT('',(-111.529994481957,122.937359864767,-81.0106744903897));
#4860=CARTESIAN_POINT('',(-111.529994481957,122.937359864767,-81.0106744903897));
#4861=CARTESIAN_POINT('Ctrl Pts',(-111.529994481957,122.930969193824,-81.0106744903897));
#4862=CARTESIAN_POINT('Ctrl Pts',(-111.529994481957,124.224440992555,-81.0106744903897));
#4863=CARTESIAN_POINT('Ctrl Pts',(-111.850631939497,122.930969193824,-81.1957946128129));
#4864=CARTESIAN_POINT('Ctrl Pts',(-111.850631939497,124.224440992555,-81.1957946128129));
#4865=CARTESIAN_POINT('Ctrl Pts',(-112.595893637265,122.930969193824,-81.3855792709696));
#4866=CARTESIAN_POINT('Ctrl Pts',(-112.595893637265,124.224440992555,-81.3855792709696));
#4867=CARTESIAN_POINT('Ctrl Pts',(-113.856111715799,122.930969193824,-81.0858699693662));
#4868=CARTESIAN_POINT('Ctrl Pts',(-113.856111715799,124.224440992555,-81.0858699693662));
#4869=CARTESIAN_POINT('Ctrl Pts',(-115.066649862454,122.930969193824,-80.2473165597762));
#4870=CARTESIAN_POINT('Ctrl Pts',(-115.066649862454,124.224440992555,-80.2473165597762));
#4871=CARTESIAN_POINT('Ctrl Pts',(-116.043255168468,122.930969193824,-78.9976046091529));
#4872=CARTESIAN_POINT('Ctrl Pts',(-116.043255168468,124.224440992555,-78.9976046091529));
#4873=CARTESIAN_POINT('Ctrl Pts',(-116.637234812114,122.930969193824,-77.5269836293621));
#4874=CARTESIAN_POINT('Ctrl Pts',(-116.637234812114,124.224440992555,-77.5269836293621));
#4875=CARTESIAN_POINT('Ctrl Pts',(-116.758174293921,122.930969193824,-76.0593501373141));
#4876=CARTESIAN_POINT('Ctrl Pts',(-116.758174293921,124.224440992555,-76.0593501373141));
#4877=CARTESIAN_POINT('Ctrl Pts',(-116.387621123593,122.930969193824,-74.8181146161938));
#4878=CARTESIAN_POINT('Ctrl Pts',(-116.387621123593,124.224440992555,-74.8181146161938));
#4879=CARTESIAN_POINT('Ctrl Pts',(-115.850631939497,122.930969193824,-74.2675913825374));
#4880=CARTESIAN_POINT('Ctrl Pts',(-115.850631939497,124.224440992555,-74.2675913825374));
#4881=CARTESIAN_POINT('Ctrl Pts',(-115.529994481957,122.930969193824,-74.0824712601142));
#4882=CARTESIAN_POINT('Ctrl Pts',(-115.529994481957,124.224440992555,-74.0824712601142));
#4883=CARTESIAN_POINT('Ctrl Pts',(-111.529994481957,122.937359864767,-81.0106744903897));
#4884=CARTESIAN_POINT('Ctrl Pts',(-111.655985564703,122.937359864767,-81.0834154759286));
#4885=CARTESIAN_POINT('Ctrl Pts',(-111.789124566157,122.941999166342,-81.1417276437762));
#4886=CARTESIAN_POINT('Ctrl Pts',(-112.132055648316,122.963800802529,-81.2508717728567));
#4887=CARTESIAN_POINT('Ctrl Pts',(-112.344262065112,122.985642902608,-81.2836304965519));
#4888=CARTESIAN_POINT('Ctrl Pts',(-112.890185001658,123.055781639719,-81.2942385303482));
#4889=CARTESIAN_POINT('Ctrl Pts',(-113.222304091371,123.111288356191,-81.2310605511146));
#4890=CARTESIAN_POINT('Ctrl Pts',(-114.040071204807,123.254369388729,-80.9469153854904));
#4891=CARTESIAN_POINT('Ctrl Pts',(-114.507617463249,123.341916036999,-80.64733737895));
#4892=CARTESIAN_POINT('Ctrl Pts',(-115.174813131733,123.441390970383,-80.050767705693));
#4893=CARTESIAN_POINT('Ctrl Pts',(-115.415868442681,123.470261290121,-79.7826739036937));
#4894=CARTESIAN_POINT('Ctrl Pts',(-115.755003463233,123.495239476746,-79.3250674771333));
#4895=CARTESIAN_POINT('Ctrl Pts',(-115.872462661464,123.49998997396,-79.1461011463315));
#4896=CARTESIAN_POINT('Ctrl Pts',(-116.085775238015,123.500009989414,-78.7767368883965));
#4897=CARTESIAN_POINT('Ctrl Pts',(-116.182038306449,123.495284034831,-78.5856508621904));
#4898=CARTESIAN_POINT('Ctrl Pts',(-116.408570505306,123.47040914673,-78.0640352851986));
#4899=CARTESIAN_POINT('Ctrl Pts',(-116.52014584973,123.4416707474,-77.7220494143149));
#4900=CARTESIAN_POINT('Ctrl Pts',(-116.700435952419,123.344280060835,-76.8627043141552));
#4901=CARTESIAN_POINT('Ctrl Pts',(-116.72827833538,123.260349185246,-76.3253510567926));
#4902=CARTESIAN_POINT('Ctrl Pts',(-116.580959608512,123.119417363555,-75.4852207472909));
#4903=CARTESIAN_POINT('Ctrl Pts',(-116.473976785389,123.063000944788,-75.16186977102));
#4904=CARTESIAN_POINT('Ctrl Pts',(-116.194331351315,122.989309527258,-74.6783741194887));
#4905=CARTESIAN_POINT('Ctrl Pts',(-116.055391044604,122.965592809847,-74.5005585112936));
#4906=CARTESIAN_POINT('Ctrl Pts',(-115.831958999688,122.946686478982,-74.2944546113625));
#4907=CARTESIAN_POINT('Ctrl Pts',(-115.771332129154,122.942999951482,-74.2445494425702));
#4908=CARTESIAN_POINT('Ctrl Pts',(-115.650653287831,122.938455031077,-74.1565333304243));
#4909=CARTESIAN_POINT('Ctrl Pts',(-115.591330433288,122.937359864766,-74.1178835881261));
#4910=CARTESIAN_POINT('Ctrl Pts',(-115.529994481957,122.937359864766,-74.0824712601142));
#4911=CARTESIAN_POINT('Origin',(-119.078493020361,109.,-80.7499999999988));
#4912=CARTESIAN_POINT('Origin',(-141.995606772677,139.904097174214,-47.6260732918001));
#4913=CARTESIAN_POINT('',(-111.835491639576,108.363035329266,-93.2952463908106));
#4914=CARTESIAN_POINT('Origin',(-145.341293669985,128.314297789504,-41.8311735994448));
#4915=CARTESIAN_POINT('',(-115.181178536884,96.7732359445553,-87.5003466984555));
#4916=CARTESIAN_POINT('Origin',(-134.275197369886,137.573299096998,-41.6148274600336));
#4917=CARTESIAN_POINT('',(-106.49494062967,105.495421682756,-89.7316435813967));
#4918=CARTESIAN_POINT('',(-106.49494062967,105.495421682756,-89.7316435813967));
#4919=CARTESIAN_POINT('',(-106.49494062967,105.495421682756,-89.7316435813966));
#4920=CARTESIAN_POINT('Origin',(-136.275197369886,130.645095866722,-38.1507258448956));
#4921=CARTESIAN_POINT('',(-108.494940629669,98.5672184524796,-86.2675419662591));
#4922=CARTESIAN_POINT('',(-108.494940629669,98.5672184524796,-86.2675419662591));
#4923=CARTESIAN_POINT('',(-108.494940629669,98.5672184524797,-86.2675419662591));
#4924=CARTESIAN_POINT('Ctrl Pts',(-108.497707871361,98.5704137879512,-86.2627489630519));
#4925=CARTESIAN_POINT('Ctrl Pts',(-107.937618152971,97.9236778885854,-87.2328528121005));
#4926=CARTESIAN_POINT('Ctrl Pts',(-108.818345328902,98.5704137879512,-86.4478690854752));
#4927=CARTESIAN_POINT('Ctrl Pts',(-108.258255610512,97.9236778885854,-87.4179729345238));
#4928=CARTESIAN_POINT('Ctrl Pts',(-109.407402641416,98.750783075701,-86.9082076752565));
#4929=CARTESIAN_POINT('Ctrl Pts',(-108.847312923026,98.1040471763352,-87.8783115243051));
#4930=CARTESIAN_POINT('Ctrl Pts',(-110.000372038795,99.5212554870629,-87.7642069906961));
#4931=CARTESIAN_POINT('Ctrl Pts',(-109.440282320405,98.8745195876971,-88.7343108397447));
#4932=CARTESIAN_POINT('Ctrl Pts',(-110.212301964103,100.674348937882,-88.6552937573345));
#4933=CARTESIAN_POINT('Ctrl Pts',(-109.652212245713,100.027613038516,-89.6253976063831));
#4934=CARTESIAN_POINT('Ctrl Pts',(-110.010968557873,102.034515403089,-89.4458315045219));
#4935=CARTESIAN_POINT('Ctrl Pts',(-109.450878839483,101.387779503723,-90.4159353535705));
#4936=CARTESIAN_POINT('Ctrl Pts',(-109.427009489273,103.394681868296,-90.0154602225416));
#4937=CARTESIAN_POINT('Ctrl Pts',(-108.866919770883,102.74794596893,-90.9855640715902));
#4938=CARTESIAN_POINT('Ctrl Pts',(-108.549340749734,104.547775319115,-90.2774669067221));
#4939=CARTESIAN_POINT('Ctrl Pts',(-107.989251031344,103.901039419749,-91.2475707557707));
#4940=CARTESIAN_POINT('Ctrl Pts',(-107.511538898252,105.318247730477,-90.1919400026446));
#4941=CARTESIAN_POINT('Ctrl Pts',(-106.951449179862,104.671511831111,-91.1620438516932));
#4942=CARTESIAN_POINT('Ctrl Pts',(-106.818345328902,105.498617018227,-89.9119707006131));
#4943=CARTESIAN_POINT('Ctrl Pts',(-106.258255610512,104.851881118861,-90.8820745496617));
#4944=CARTESIAN_POINT('Ctrl Pts',(-106.497707871361,105.498617018227,-89.7268505781898));
#4945=CARTESIAN_POINT('Ctrl Pts',(-105.937618152971,104.851881118861,-90.6969544272384));
#4946=CARTESIAN_POINT('Ctrl Pts',(-108.494940629669,98.5672184524797,-86.2675419662592));
#4947=CARTESIAN_POINT('Ctrl Pts',(-108.620931712415,98.5672184524797,-86.3402829517981));
#4948=CARTESIAN_POINT('Ctrl Pts',(-108.740009575843,98.5788155545531,-86.4229497251191));
#4949=CARTESIAN_POINT('Ctrl Pts',(-109.015792308145,98.634550154098,-86.6483982077968));
#4950=CARTESIAN_POINT('Ctrl Pts',(-109.160240827059,98.6909481351825,-86.7985170532378));
#4951=CARTESIAN_POINT('Ctrl Pts',(-109.477961818401,98.884314307059,-87.2043824505149));
#4952=CARTESIAN_POINT('Ctrl Pts',(-109.620465834967,99.047756217635,-87.4696274118531));
#4953=CARTESIAN_POINT('Ctrl Pts',(-109.88505667753,99.5434281228911,-88.1436116529208));
#4954=CARTESIAN_POINT('Ctrl Pts',(-109.944782655288,99.9267917722889,-88.5503990928816));
#4955=CARTESIAN_POINT('Ctrl Pts',(-109.931222669289,100.613385759641,-89.132932800729));
#4956=CARTESIAN_POINT('Ctrl Pts',(-109.895248991132,100.904400962771,-89.3446672830305));
#4957=CARTESIAN_POINT('Ctrl Pts',(-109.799168414145,101.381966460934,-89.6408763836526));
#4958=CARTESIAN_POINT('Ctrl Pts',(-109.754281345734,101.564677285217,-89.7431020350957));
#4959=CARTESIAN_POINT('Ctrl Pts',(-109.647683916166,101.93405752606,-89.9278381616077));
#4960=CARTESIAN_POINT('Ctrl Pts',(-109.585780717548,102.121418154361,-90.0107041459795));
#4961=CARTESIAN_POINT('Ctrl Pts',(-109.399335228826,102.623158600648,-90.2043869062662));
#4962=CARTESIAN_POINT('Ctrl Pts',(-109.259387572093,102.942330744829,-90.2980516526588));
#4963=CARTESIAN_POINT('Ctrl Pts',(-108.856079275086,103.713602817721,-90.4495286319902));
#4964=CARTESIAN_POINT('Ctrl Pts',(-108.560802720886,104.170639304011,-90.4718337906789));
#4965=CARTESIAN_POINT('Ctrl Pts',(-107.984073142598,104.807412067022,-90.3754648931577));
#4966=CARTESIAN_POINT('Ctrl Pts',(-107.731615284225,105.031808587313,-90.3040840691712));
#4967=CARTESIAN_POINT('Ctrl Pts',(-107.274706570105,105.310186009746,-90.1276174249943));
#4968=CARTESIAN_POINT('Ctrl Pts',(-107.082643892882,105.395243156987,-90.0418124615454));
#4969=CARTESIAN_POINT('Ctrl Pts',(-106.81731713635,105.462525333909,-89.9082723306999));
#4970=CARTESIAN_POINT('Ctrl Pts',(-106.748607297535,105.475545269237,-89.8723672736483));
#4971=CARTESIAN_POINT('Ctrl Pts',(-106.617982888177,105.491574342406,-89.8015773906488));
#4972=CARTESIAN_POINT('Ctrl Pts',(-106.556276581001,105.495421682755,-89.7670559094086));
#4973=CARTESIAN_POINT('Ctrl Pts',(-106.49494062967,105.495421682755,-89.7316435813966));
#4974=CARTESIAN_POINT('Origin',(-119.078493020361,109.,-80.7499999999988));
#4975=CARTESIAN_POINT('Origin',(-98.8802009968175,127.881285087611,-122.304146684539));
#4976=CARTESIAN_POINT('',(-122.975807503838,96.7732359445554,-73.9996533015419));
#4977=CARTESIAN_POINT('Origin',(-102.225887894125,139.471084472322,-116.509246992184));
#4978=CARTESIAN_POINT('',(-126.321494401146,108.363035329266,-68.2047536091869));
#4979=CARTESIAN_POINT('Origin',(-91.1597915940262,130.212083164828,-116.292900852773));
#4980=CARTESIAN_POINT('',(-118.565048334243,98.5672184524784,-68.8256037842474));
#4981=CARTESIAN_POINT('',(-118.565048334243,98.5672184524783,-68.8256037842474));
#4982=CARTESIAN_POINT('',(-118.565048334243,98.5672184524784,-68.8256037842474));
#4983=CARTESIAN_POINT('Origin',(-93.159791594026,137.140286395103,-112.828799237635));
#4984=CARTESIAN_POINT('',(-120.565048334243,105.495421682754,-65.3615021691091));
#4985=CARTESIAN_POINT('',(-120.565048334243,105.495421682754,-65.3615021691091));
#4986=CARTESIAN_POINT('',(-120.565048334243,105.495421682754,-65.3615021691091));
#4987=CARTESIAN_POINT('Ctrl Pts',(-120.562281092551,105.498617018225,-65.3662951723163));
#4988=CARTESIAN_POINT('Ctrl Pts',(-121.122370810941,104.85188111886,-64.3961913232677));
#4989=CARTESIAN_POINT('Ctrl Pts',(-120.882918550091,105.498617018225,-65.5514152947396));
#4990=CARTESIAN_POINT('Ctrl Pts',(-121.443008268481,104.85188111886,-64.581311445691));
#4991=CARTESIAN_POINT('Ctrl Pts',(-121.471975862605,105.318247730476,-66.0117538845209));
#4992=CARTESIAN_POINT('Ctrl Pts',(-122.032065580995,104.67151183111,-65.0416500354723));
#4993=CARTESIAN_POINT('Ctrl Pts',(-122.064945259985,104.547775319114,-66.8677531999604));
#4994=CARTESIAN_POINT('Ctrl Pts',(-122.625034978375,103.901039419748,-65.8976493509118));
#4995=CARTESIAN_POINT('Ctrl Pts',(-122.276875185293,103.394681868295,-67.7588399665989));
#4996=CARTESIAN_POINT('Ctrl Pts',(-122.836964903683,102.747945968929,-66.7887361175503));
#4997=CARTESIAN_POINT('Ctrl Pts',(-122.075541779062,102.034515403088,-68.5493777137862));
#4998=CARTESIAN_POINT('Ctrl Pts',(-122.635631497452,101.387779503722,-67.5792738647376));
#4999=CARTESIAN_POINT('Ctrl Pts',(-121.491582710463,100.674348937881,-69.1190064318059));
#5000=CARTESIAN_POINT('Ctrl Pts',(-122.051672428853,100.027613038515,-68.1489025827573));
#5001=CARTESIAN_POINT('Ctrl Pts',(-120.613913970924,99.5212554870615,-69.3810131159864));
#5002=CARTESIAN_POINT('Ctrl Pts',(-121.174003689314,98.8745195876958,-68.4109092669378));
#5003=CARTESIAN_POINT('Ctrl Pts',(-119.576112119442,98.7507830756997,-69.2954862119089));
#5004=CARTESIAN_POINT('Ctrl Pts',(-120.136201837832,98.104047176334,-68.3253823628603));
#5005=CARTESIAN_POINT('Ctrl Pts',(-118.882918550091,98.5704137879498,-69.0155169098773));
#5006=CARTESIAN_POINT('Ctrl Pts',(-119.443008268481,97.9236778885841,-68.0454130608287));
#5007=CARTESIAN_POINT('Ctrl Pts',(-118.562281092551,98.5704137879498,-68.8303967874541));
#5008=CARTESIAN_POINT('Ctrl Pts',(-119.122370810941,97.9236778885841,-67.8602929384055));
#5009=CARTESIAN_POINT('Ctrl Pts',(-120.565048334243,105.495421682754,-65.3615021691091));
#5010=CARTESIAN_POINT('Ctrl Pts',(-120.691039416989,105.495421682754,-65.4342431546481));
#5011=CARTESIAN_POINT('Ctrl Pts',(-120.814135033437,105.479185279105,-65.509950975606));
#5012=CARTESIAN_POINT('Ctrl Pts',(-121.108798536521,105.401649043373,-65.7026970040038));
#5013=CARTESIAN_POINT('Ctrl Pts',(-121.272162868975,105.32340896221,-65.8200526993256));
#5014=CARTESIAN_POINT('Ctrl Pts',(-121.650625788444,105.059904053223,-66.1207099909364));
#5015=CARTESIAN_POINT('Ctrl Pts',(-121.841200031555,104.840955426175,-66.3026948775666));
#5016=CARTESIAN_POINT('Ctrl Pts',(-122.229702683097,104.20220248838,-66.7620575698267));
#5017=CARTESIAN_POINT('Ctrl Pts',(-122.365246282272,103.731292190713,-67.0375250373832));
#5018=CARTESIAN_POINT('Ctrl Pts',(-122.437834115624,102.945223269976,-67.4708463451536));
#5019=CARTESIAN_POINT('Ctrl Pts',(-122.426862867774,102.625337747109,-67.6392753478494));
#5020=CARTESIAN_POINT('Ctrl Pts',(-122.352414034946,102.122794062321,-67.8980171685339));
#5021=CARTESIAN_POINT('Ctrl Pts',(-122.311641017802,101.935332740824,-67.9931170741559));
#5022=CARTESIAN_POINT('Ctrl Pts',(-122.205060922126,101.565932484526,-68.1778231774862));
#5023=CARTESIAN_POINT('Ctrl Pts',(-122.139064926783,101.383297810808,-68.2677780937319));
#5024=CARTESIAN_POINT('Ctrl Pts',(-121.931077153049,100.906432252622,-68.4987731861706));
#5025=CARTESIAN_POINT('Ctrl Pts',(-121.766241312432,100.615998507772,-68.6355455315589));
#5026=CARTESIAN_POINT('Ctrl Pts',(-121.278590206767,99.9421171214444,-68.9331085407376));
#5027=CARTESIAN_POINT('Ctrl Pts',(-120.910627382145,99.5690115107432,-69.0813100128094));
#5028=CARTESIAN_POINT('Ctrl Pts',(-120.211847266071,99.0731705694225,-69.1963388478251));
#5029=CARTESIAN_POINT('Ctrl Pts',(-119.910531355856,98.9051904678996,-69.2095826519892));
#5030=CARTESIAN_POINT('Ctrl Pts',(-119.389804002114,98.7005044629965,-69.1436531341076));
#5031=CARTESIAN_POINT('Ctrl Pts',(-119.177202045119,98.6391640331656,-69.0934232467741));
#5032=CARTESIAN_POINT('Ctrl Pts',(-118.895501925765,98.5907881871084,-68.988242612226));
#5033=CARTESIAN_POINT('Ctrl Pts',(-118.823599460482,98.5814547792815,-68.9578673464248));
#5034=CARTESIAN_POINT('Ctrl Pts',(-118.689039034596,98.5699706265173,-68.8938948440334));
#5035=CARTESIAN_POINT('Ctrl Pts',(-118.626384285574,98.5672184524785,-68.8610161122592));
#5036=CARTESIAN_POINT('Ctrl Pts',(-118.565048334243,98.5672184524785,-68.8256037842472));
#5037=CARTESIAN_POINT('Origin',(-119.078493020361,109.,-80.7499999999988));
#5038=CARTESIAN_POINT('Origin',(-69.3034604663987,124.991664350565,-51.4350212868557));
#5039=CARTESIAN_POINT('',(-67.366968793295,124.991664350565,-50.3169872981059));
#5040=CARTESIAN_POINT('Origin',(-68.8034604663987,123.191664350565,-52.3010466906402));
#5041=CARTESIAN_POINT('',(-66.866968793295,124.991664350565,-51.1830127018903));
#5042=CARTESIAN_POINT('Origin',(-69.3034604663987,124.991664350565,-51.4350212868557));
#5043=CARTESIAN_POINT('Origin',(-76.346812504256,100.571155122824,-40.3758635351318));
#5044=CARTESIAN_POINT('',(-73.9165625814855,100.571155122824,-38.9727580880221));
#5045=CARTESIAN_POINT('Origin',(-75.81738964085,102.337180526609,-41.2928508332395));
#5046=CARTESIAN_POINT('',(-74.1665625814855,101.437180526609,-38.5397453861299));
#5047=CARTESIAN_POINT('Origin',(-76.346812504256,100.571155122824,-40.3758635351318));
#5048=CARTESIAN_POINT('Origin',(-62.497624927873,101.437180526611,-64.3633600609793));
#5049=CARTESIAN_POINT('',(-60.0673750051025,101.437180526611,-62.9602546138697));
#5050=CARTESIAN_POINT('Origin',(-63.527047791279,101.471155122826,-62.580347359087));
#5051=CARTESIAN_POINT('',(-60.3173750051025,100.571155122826,-62.5272419119774));
#5052=CARTESIAN_POINT('Origin',(-62.497624927873,101.437180526611,-64.3633600609793));
#5053=CARTESIAN_POINT('',(0.,0.,0.));
#5054=CARTESIAN_POINT('Origin',(-116.12807069331,130.343145750508,-79.0465728752519));
#5055=CARTESIAN_POINT('',(-115.553844652019,135.790187558086,-80.460786437625));
#5056=CARTESIAN_POINT('Origin',(-118.577560436093,133.171572875254,-80.460786437625));
#5057=CARTESIAN_POINT('',(-113.104354909236,132.96176043334,-79.0465728752519));
#5058=CARTESIAN_POINT('',(-113.104354909236,132.96176043334,-79.0465728752519));
#5059=CARTESIAN_POINT('Origin',(-116.12807069331,130.343145750508,-79.0465728752519));
#5060=CARTESIAN_POINT('Origin',(-116.12807069331,130.343145750508,-79.0465728752519));
#5061=CARTESIAN_POINT('',(-113.482319382245,132.634433597986,-79.0465728752519));
#5062=CARTESIAN_POINT('Origin',(-116.12807069331,130.343145750508,-79.0465728752519));
#5063=CARTESIAN_POINT('Origin',(-118.577560436093,133.171572875254,-80.460786437625));
#5064=CARTESIAN_POINT('',(-117.21688833326,134.349949482528,-80.460786437625));
#5065=CARTESIAN_POINT('Origin',(-118.577560436093,133.171572875254,-80.460786437625));
#5066=CARTESIAN_POINT('Origin',(-118.577560436093,133.171572875254,-80.460786437625));
#5067=CARTESIAN_POINT('',(-113.610617334806,128.811013710585,-77.9859127034721));
#5068=CARTESIAN_POINT('Origin',(-114.290953386223,128.221825406948,-77.9859127034721));
#5069=CARTESIAN_POINT('',(-117.34608919255,133.124365075823,-80.1425883860911));
#5070=CARTESIAN_POINT('',(-117.897224384677,133.760761178891,-80.460786437625));
#5071=CARTESIAN_POINT('Origin',(-118.026425243967,132.535176772186,-80.1425883860911));
#5072=CARTESIAN_POINT('Origin',(-118.577560436093,133.171572875254,-80.460786437625));
#5073=CARTESIAN_POINT('',(-117.21688833326,134.349949482528,-80.460786437625));
#5074=CARTESIAN_POINT('Origin',(-114.290953386223,128.221825406948,-77.9859127034721));
#5075=CARTESIAN_POINT('',(-111.645202075158,130.513113254426,-77.9859127034721));
#5076=CARTESIAN_POINT('Origin',(-114.290953386223,128.221825406948,-77.9859127034721));
#5077=CARTESIAN_POINT('Origin',(-114.290953386223,128.221825406948,-77.9859127034721));
#5078=CARTESIAN_POINT('',(-111.645202075158,130.513113254426,-77.9859127034721));
#5079=CARTESIAN_POINT('',(0.,0.,0.));
#5080=CARTESIAN_POINT('Origin',(-102.211351574804,130.535898384862,-71.0117513459462));
#5081=CARTESIAN_POINT('',(-100.365693618373,135.788854382,-72.0117513459462));
#5082=CARTESIAN_POINT('Origin',(-103.943402382373,134.,-72.0117513459462));
#5083=CARTESIAN_POINT('',(-98.6336428108046,132.324752766862,-71.0117513459462));
#5084=CARTESIAN_POINT('',(-98.6336428108046,132.324752766862,-71.0117513459462));
#5085=CARTESIAN_POINT('Origin',(-102.211351574804,130.535898384862,-71.0117513459462));
#5086=CARTESIAN_POINT('Origin',(-102.211351574804,130.535898384862,-71.0117513459462));
#5087=CARTESIAN_POINT('',(-99.0808564063046,132.101145969112,-71.0117513459462));
#5088=CARTESIAN_POINT('Origin',(-102.211351574804,130.535898384862,-71.0117513459462));
#5089=CARTESIAN_POINT('Origin',(-103.943402382373,134.,-72.0117513459462));
#5090=CARTESIAN_POINT('',(-102.333433438573,134.8049844719,-72.0117513459462));
#5091=CARTESIAN_POINT('Origin',(-103.943402382373,134.,-72.0117513459462));
#5092=CARTESIAN_POINT('Origin',(-103.943402382373,134.,-72.0117513459462));
#5093=CARTESIAN_POINT('',(-100.107328997228,128.340314409459,-70.2617513459462));
#5094=CARTESIAN_POINT('Origin',(-100.912313469128,127.937822173509,-70.2617513459462));
#5095=CARTESIAN_POINT('',(-102.74870647877,133.623069372544,-71.7867513459462));
#5096=CARTESIAN_POINT('',(-103.138417910473,134.40249223595,-72.0117513459462));
#5097=CARTESIAN_POINT('Origin',(-103.55369095067,133.220577136594,-71.7867513459462));
#5098=CARTESIAN_POINT('Origin',(-103.943402382373,134.,-72.0117513459462));
#5099=CARTESIAN_POINT('',(-102.333433438573,134.8049844719,-72.0117513459462));
#5100=CARTESIAN_POINT('Origin',(-100.912313469128,127.937822173509,-70.2617513459462));
#5101=CARTESIAN_POINT('',(-97.7818183006279,129.503069757759,-70.2617513459462));
#5102=CARTESIAN_POINT('Origin',(-100.912313469128,127.937822173509,-70.2617513459462));
#5103=CARTESIAN_POINT('Origin',(-100.912313469128,127.937822173509,-70.2617513459462));
#5104=CARTESIAN_POINT('',(-97.7818183006279,129.503069757759,-70.2617513459462));
#5105=CARTESIAN_POINT('',(0.,0.,0.));
#5106=CARTESIAN_POINT('Origin',(-88.8998569762207,131.101020514434,-63.3263563561378));
#5107=CARTESIAN_POINT('',(-85.8999646576036,135.868902317108,-63.8439944463428));
#5108=CARTESIAN_POINT('Origin',(-89.7964324483888,134.96472381959,-63.8439944463428));
#5109=CARTESIAN_POINT('',(-85.0033891854356,132.005199011951,-63.3263563561378));
#5110=CARTESIAN_POINT('',(-85.0033891854356,132.005199011951,-63.3263563561378));
#5111=CARTESIAN_POINT('Origin',(-88.8998569762207,131.101020514434,-63.3263563561378));
#5112=CARTESIAN_POINT('Origin',(-88.8998569762207,131.101020514434,-63.3263563561378));
#5113=CARTESIAN_POINT('',(-85.4904476592837,131.892176699762,-63.3263563561378));
#5114=CARTESIAN_POINT('Origin',(-88.8998569762207,131.101020514434,-63.3263563561378));
#5115=CARTESIAN_POINT('Origin',(-89.7964324483888,134.96472381959,-63.8439944463428));
#5116=CARTESIAN_POINT('',(-88.0430219425354,135.371604143473,-63.8439944463428));
#5117=CARTESIAN_POINT('Origin',(-89.7964324483888,134.96472381959,-63.8439944463428));
#5118=CARTESIAN_POINT('Origin',(-89.7964324483888,134.96472381959,-63.8439944463428));
#5119=CARTESIAN_POINT('',(-87.350720119168,128.406683197508,-62.938127788484));
#5120=CARTESIAN_POINT('Origin',(-88.2274253720946,128.203243035566,-62.938127788484));
#5121=CARTESIAN_POINT('',(-88.7179977142243,134.298830737871,-63.7275258760467));
#5122=CARTESIAN_POINT('',(-88.9197271954621,135.168163981531,-63.8439944463428));
#5123=CARTESIAN_POINT('Origin',(-89.5947029671509,134.09539057593,-63.7275258760467));
#5124=CARTESIAN_POINT('Origin',(-89.7964324483888,134.96472381959,-63.8439944463428));
#5125=CARTESIAN_POINT('',(-88.0430219425354,135.371604143473,-63.8439944463428));
#5126=CARTESIAN_POINT('Origin',(-88.2274253720946,128.203243035566,-62.938127788484));
#5127=CARTESIAN_POINT('',(-84.8180160551577,128.994399220895,-62.938127788484));
#5128=CARTESIAN_POINT('Origin',(-88.2274253720946,128.203243035566,-62.938127788484));
#5129=CARTESIAN_POINT('Origin',(-88.2274253720946,128.203243035566,-62.938127788484));
#5130=CARTESIAN_POINT('',(-84.8180160551577,128.994399220895,-62.938127788484));
#5131=CARTESIAN_POINT('',(0.,0.,0.));
#5132=CARTESIAN_POINT('Origin',(-75.5607164801933,132.,-55.624999999998));
#5133=CARTESIAN_POINT('',(-75.5607164801933,136.,-59.6249999999981));
#5134=CARTESIAN_POINT('Origin',(-75.5607164801933,136.,-55.624999999998));
#5135=CARTESIAN_POINT('',(-75.5607164801933,132.,-59.6249999999981));
#5136=CARTESIAN_POINT('',(-75.5607164801933,132.,-59.6249999999981));
#5137=CARTESIAN_POINT('Origin',(-75.5607164801933,132.,-55.624999999998));
#5138=CARTESIAN_POINT('Origin',(-75.5607164801933,132.,-55.624999999998));
#5139=CARTESIAN_POINT('',(-75.5607164801933,132.,-59.1249999999981));
#5140=CARTESIAN_POINT('Origin',(-75.5607164801933,132.,-55.624999999998));
#5141=CARTESIAN_POINT('Origin',(-75.5607164801933,136.,-55.624999999998));
#5142=CARTESIAN_POINT('',(-75.5607164801933,136.,-57.424999999998));
#5143=CARTESIAN_POINT('Origin',(-75.5607164801933,136.,-55.624999999998));
#5144=CARTESIAN_POINT('Origin',(-75.5607164801933,136.,-55.624999999998));
#5145=CARTESIAN_POINT('',(-75.5607164801933,129.,-56.524999999998));
#5146=CARTESIAN_POINT('Origin',(-75.5607164801933,129.,-55.624999999998));
#5147=CARTESIAN_POINT('',(-75.5607164801933,135.1,-56.524999999998));
#5148=CARTESIAN_POINT('',(-75.5607164801933,136.,-56.524999999998));
#5149=CARTESIAN_POINT('Origin',(-75.5607164801933,135.1,-55.624999999998));
#5150=CARTESIAN_POINT('Origin',(-75.5607164801933,136.,-55.624999999998));
#5151=CARTESIAN_POINT('',(-75.5607164801933,136.,-57.424999999998));
#5152=CARTESIAN_POINT('Origin',(-75.5607164801933,129.,-55.624999999998));
#5153=CARTESIAN_POINT('',(-75.5607164801933,129.,-59.1249999999981));
#5154=CARTESIAN_POINT('Origin',(-75.5607164801933,129.,-55.624999999998));
#5155=CARTESIAN_POINT('Origin',(-75.5607164801933,129.,-55.624999999998));
#5156=CARTESIAN_POINT('',(-75.5607164801933,129.,-59.1249999999981));
#5157=CARTESIAN_POINT('',(-12.7683873876991,56.3012899998748,43.4781798467456));
#5158=CARTESIAN_POINT('',(-22.4000040844042,254.577374315256,38.728643251025));
#5159=CARTESIAN_POINT('',(-44.7393996466421,286.888929591391,-0.542249927592924));
#5160=CARTESIAN_POINT('',(-75.4310082996939,297.414432149061,-39.0811659930832));
#5161=CARTESIAN_POINT('',(-10.0317249986676,270.739548408369,-15.7797463643511));
#5162=CARTESIAN_POINT('',(-22.6769527544393,36.8799811186442,39.4637630808387));
#5163=CARTESIAN_POINT('',(43.9283203292622,145.048364335116,-137.330214690215));
#5164=CARTESIAN_POINT('',(-70.150751068712,45.7295323022975,66.908474173488));
#5165=CARTESIAN_POINT('',(16.1850811205472,103.887257875328,-162.257393485845));
#5166=CARTESIAN_POINT('',(-117.405702678433,62.3288247714053,72.3345349171988));
#5167=CARTESIAN_POINT('',(-24.6426326618715,76.7624628485525,-173.891497635406));
#5168=CARTESIAN_POINT('',(-44.5237921714637,76.7498579606653,75.7744125587609));
#5169=CARTESIAN_POINT('',(31.9506663628748,89.0163133999874,-127.215877792275));
#5170=UNCERTAINTY_MEASURE_WITH_UNIT(LENGTH_MEASURE(0.01),#5184,
'DISTANCE_ACCURACY_VALUE',
'Maximum model space distance between geometric entities at asserted c
onnectivities');
#5171=UNCERTAINTY_MEASURE_WITH_UNIT(LENGTH_MEASURE(0.01),#5184,
'DISTANCE_ACCURACY_VALUE',
'Maximum model space distance between geometric entities at asserted c
onnectivities');
#5172=UNCERTAINTY_MEASURE_WITH_UNIT(LENGTH_MEASURE(0.01),#5184,
'DISTANCE_ACCURACY_VALUE',
'Maximum model space distance between geometric entities at asserted c
onnectivities');
#5173=UNCERTAINTY_MEASURE_WITH_UNIT(LENGTH_MEASURE(0.01),#5184,
'DISTANCE_ACCURACY_VALUE',
'Maximum model space distance between geometric entities at asserted c
onnectivities');
#5174=UNCERTAINTY_MEASURE_WITH_UNIT(LENGTH_MEASURE(0.01),#5184,
'DISTANCE_ACCURACY_VALUE',
'Maximum model space distance between geometric entities at asserted c
onnectivities');
#5175=UNCERTAINTY_MEASURE_WITH_UNIT(LENGTH_MEASURE(0.01),#5184,
'DISTANCE_ACCURACY_VALUE',
'Maximum model space distance between geometric entities at asserted c
onnectivities');
#5176=UNCERTAINTY_MEASURE_WITH_UNIT(LENGTH_MEASURE(0.01),#5184,
'DISTANCE_ACCURACY_VALUE',
'Maximum model space distance between geometric entities at asserted c
onnectivities');
#5177=(
GEOMETRIC_REPRESENTATION_CONTEXT(3)
GLOBAL_UNCERTAINTY_ASSIGNED_CONTEXT((#5170))
GLOBAL_UNIT_ASSIGNED_CONTEXT((#5184,#5186,#5187))
REPRESENTATION_CONTEXT('','3D')
);
#5178=(
GEOMETRIC_REPRESENTATION_CONTEXT(3)
GLOBAL_UNCERTAINTY_ASSIGNED_CONTEXT((#5171))
GLOBAL_UNIT_ASSIGNED_CONTEXT((#5184,#5186,#5187))
REPRESENTATION_CONTEXT('','3D')
);
#5179=(
GEOMETRIC_REPRESENTATION_CONTEXT(3)
GLOBAL_UNCERTAINTY_ASSIGNED_CONTEXT((#5172))
GLOBAL_UNIT_ASSIGNED_CONTEXT((#5184,#5186,#5187))
REPRESENTATION_CONTEXT('','3D')
);
#5180=(
GEOMETRIC_REPRESENTATION_CONTEXT(3)
GLOBAL_UNCERTAINTY_ASSIGNED_CONTEXT((#5173))
GLOBAL_UNIT_ASSIGNED_CONTEXT((#5184,#5186,#5187))
REPRESENTATION_CONTEXT('','3D')
);
#5181=(
GEOMETRIC_REPRESENTATION_CONTEXT(3)
GLOBAL_UNCERTAINTY_ASSIGNED_CONTEXT((#5174))
GLOBAL_UNIT_ASSIGNED_CONTEXT((#5184,#5186,#5187))
REPRESENTATION_CONTEXT('','3D')
);
#5182=(
GEOMETRIC_REPRESENTATION_CONTEXT(3)
GLOBAL_UNCERTAINTY_ASSIGNED_CONTEXT((#5175))
GLOBAL_UNIT_ASSIGNED_CONTEXT((#5184,#5186,#5187))
REPRESENTATION_CONTEXT('','3D')
);
#5183=(
GEOMETRIC_REPRESENTATION_CONTEXT(3)
GLOBAL_UNCERTAINTY_ASSIGNED_CONTEXT((#5176))
GLOBAL_UNIT_ASSIGNED_CONTEXT((#5184,#5186,#5187))
REPRESENTATION_CONTEXT('','3D')
);
#5184=(
LENGTH_UNIT()
NAMED_UNIT(*)
SI_UNIT(.MILLI.,.METRE.)
);
#5185=(
LENGTH_UNIT()
NAMED_UNIT(*)
SI_UNIT($,.METRE.)
);
#5186=(
NAMED_UNIT(*)
PLANE_ANGLE_UNIT()
SI_UNIT($,.RADIAN.)
);
#5187=(
NAMED_UNIT(*)
SI_UNIT($,.STERADIAN.)
SOLID_ANGLE_UNIT()
);
#5188=SHAPE_DEFINITION_REPRESENTATION(#5194,#5213);
#5189=SHAPE_DEFINITION_REPRESENTATION(#5195,#5214);
#5190=SHAPE_DEFINITION_REPRESENTATION(#5196,#5215);
#5191=SHAPE_DEFINITION_REPRESENTATION(#5197,#5216);
#5192=SHAPE_DEFINITION_REPRESENTATION(#5198,#5217);
#5193=SHAPE_DEFINITION_REPRESENTATION(#5199,#5218);
#5194=PRODUCT_DEFINITION_SHAPE('',$,#5220);
#5195=PRODUCT_DEFINITION_SHAPE('',$,#5221);
#5196=PRODUCT_DEFINITION_SHAPE('',$,#5222);
#5197=PRODUCT_DEFINITION_SHAPE('',$,#5223);
#5198=PRODUCT_DEFINITION_SHAPE('',$,#5224);
#5199=PRODUCT_DEFINITION_SHAPE('',$,#5225);
#5200=PRODUCT_DEFINITION_SHAPE($,$,#50);
#5201=PRODUCT_DEFINITION_SHAPE($,$,#51);
#5202=PRODUCT_DEFINITION_SHAPE($,$,#52);
#5203=PRODUCT_DEFINITION_SHAPE($,$,#53);
#5204=PRODUCT_DEFINITION_SHAPE($,$,#54);
#5205=PRODUCT_DEFINITION_SHAPE($,$,#55);
#5206=PRODUCT_DEFINITION_SHAPE($,$,#56);
#5207=PRODUCT_DEFINITION_SHAPE($,$,#57);
#5208=PRODUCT_DEFINITION_SHAPE($,$,#58);
#5209=PRODUCT_DEFINITION_SHAPE($,$,#59);
#5210=PRODUCT_DEFINITION_SHAPE($,$,#60);
#5211=PRODUCT_DEFINITION_SHAPE($,$,#61);
#5212=PRODUCT_DEFINITION_SHAPE($,$,#62);
#5213=SHAPE_REPRESENTATION('',(#2424,#2665,#2666,#2667,#2668,#2669,#2670,
#2671,#2672,#2673,#2674,#2675,#2676,#2677),#5177);
#5214=SHAPE_REPRESENTATION('',(#2425),#5178);
#5215=SHAPE_REPRESENTATION('',(#2605),#5179);
#5216=SHAPE_REPRESENTATION('',(#2620),#5180);
#5217=SHAPE_REPRESENTATION('',(#2635),#5181);
#5218=SHAPE_REPRESENTATION('',(#2650),#5182);
#5219=PRODUCT_DEFINITION_CONTEXT('part definition',#5239,'design');
#5220=PRODUCT_DEFINITION('2026-10-24-10-25-28-847',
'MAT-072',#5226,#5219);
#5221=PRODUCT_DEFINITION('Sprinkler','Sprinkler',#5227,#5219);
#5222=PRODUCT_DEFINITION('Nozzle 45','Nozzle 45',#5228,#5219);
#5223=PRODUCT_DEFINITION('Nozzle 60','Nozzle 60',#5229,#5219);
#5224=PRODUCT_DEFINITION('Nozzle 75','Nozzle 75',#5230,#5219);
#5225=PRODUCT_DEFINITION('Nozzle 90','Nozzle 90',#5231,#5219);
#5226=PRODUCT_DEFINITION_FORMATION('',$,#5241);
#5227=PRODUCT_DEFINITION_FORMATION('',$,#5242);
#5228=PRODUCT_DEFINITION_FORMATION('',$,#5243);
#5229=PRODUCT_DEFINITION_FORMATION('',$,#5244);
#5230=PRODUCT_DEFINITION_FORMATION('',$,#5245);
#5231=PRODUCT_DEFINITION_FORMATION('',$,#5246);
#5232=PRODUCT_RELATED_PRODUCT_CATEGORY(
'MAT-072',
'MAT-072',(#5241));
#5233=PRODUCT_RELATED_PRODUCT_CATEGORY('Sprinkler','Sprinkler',(#5242));
#5234=PRODUCT_RELATED_PRODUCT_CATEGORY('Nozzle 45','Nozzle 45',(#5243));
#5235=PRODUCT_RELATED_PRODUCT_CATEGORY('Nozzle 60','Nozzle 60',(#5244));
#5236=PRODUCT_RELATED_PRODUCT_CATEGORY('Nozzle 75','Nozzle 75',(#5245));
#5237=PRODUCT_RELATED_PRODUCT_CATEGORY('Nozzle 90','Nozzle 90',(#5246));
#5238=APPLICATION_PROTOCOL_DEFINITION('international standard',
'automotive_design',2009,#5239);
#5239=APPLICATION_CONTEXT(
'Core Data for Automotive Mechanical Design Process');
#5240=PRODUCT_CONTEXT('part definition',#5239,'mechanical');
#5241=PRODUCT('2026-10-24-10-25-28-847',
'MAT-072',$,(#5240));
#5242=PRODUCT('Sprinkler','Sprinkler',$,(#5240));
#5243=PRODUCT('Nozzle 45','Nozzle 45',$,(#5240));
#5244=PRODUCT('Nozzle 60','Nozzle 60',$,(#5240));
#5245=PRODUCT('Nozzle 75','Nozzle 75',$,(#5240));
#5246=PRODUCT('Nozzle 90','Nozzle 90',$,(#5240));
#5247=PRESENTATION_STYLE_ASSIGNMENT((#5248));
#5248=SURFACE_STYLE_USAGE(.BOTH.,#5249);
#5249=SURFACE_SIDE_STYLE('',(#5250));
#5250=SURFACE_STYLE_FILL_AREA(#5251);
#5251=FILL_AREA_STYLE('Steel - Satin',(#5252));
#5252=FILL_AREA_STYLE_COLOUR('Steel - Satin',#5253);
#5253=COLOUR_RGB('Steel - Satin',0.627450980392157,0.627450980392157,0.627450980392157);
ENDSEC;
END-ISO-10303-21;
